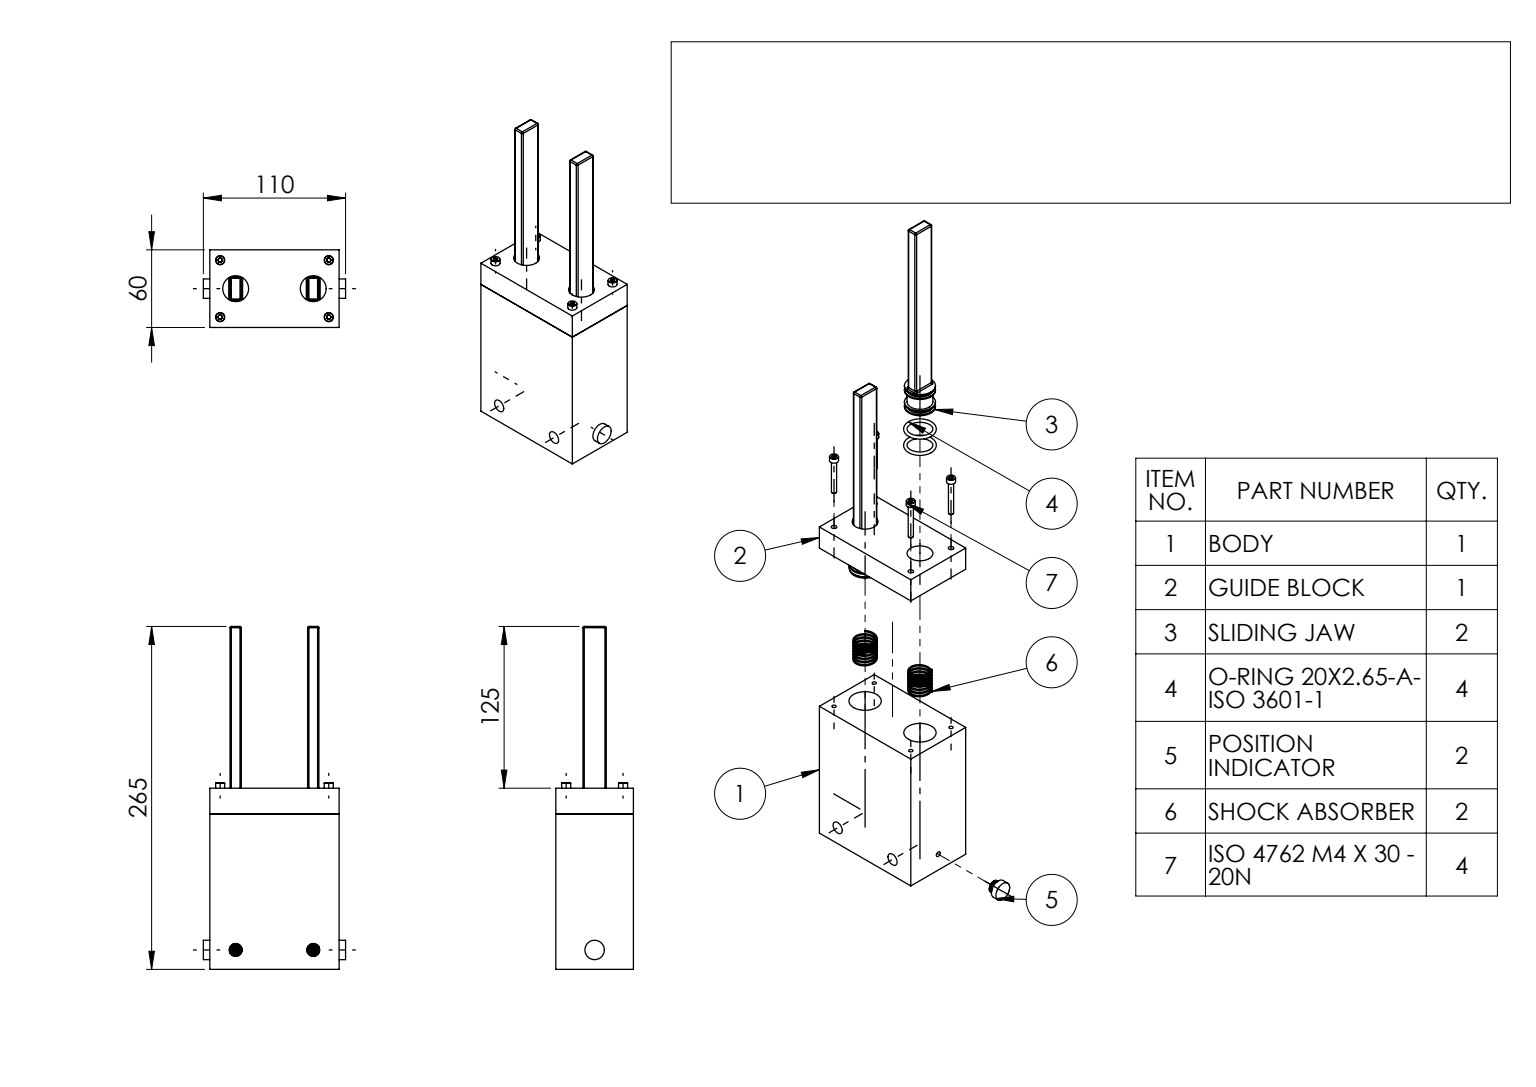
ISO-10303-21;
HEADER;
FILE_DESCRIPTION (('STEP AP214'),
    '1' );
FILE_NAME ('BR-006',
    '2026-09-29T11:11:29',
    ( '' ),
    ( '' ),
    'SwSTEP 2.0',
    'SolidWorks 2026',
    '' );
FILE_SCHEMA (( 'AUTOMOTIVE_DESIGN' ));
ENDSEC;

DATA;
#1 = EDGE_CURVE ( 'NONE', #3439, #1476, #1309, .T. ) ;
#2 = DIRECTION ( 'NONE',  ( 6.123233995736766036E-17, -1.000000000000000000, 0.000000000000000000 ) ) ;
#3 = AXIS2_PLACEMENT_3D ( 'NONE', #1406, #4531, #6990 ) ;
#4 = ORIENTED_EDGE ( 'NONE', *, *, #636, .F. ) ;
#5 = CARTESIAN_POINT ( 'NONE',  ( 42.00000000000000711, 48.00000000000002842, -23.64999999999992042 ) ) ;
#6 = CARTESIAN_POINT ( 'NONE',  ( -39.38303923565386100, -41.70000000000000995, -1.486127417882099788 ) ) ;
#7 = CARTESIAN_POINT ( 'NONE',  ( -22.03669253526174998, -31.34999999999999787, 4.057507815433014642 ) ) ;
#8 = ADVANCED_FACE ( 'NONE', ( #3264 ), #5944, .F. ) ;
#9 = FACE_BOUND ( 'NONE', #6715, .T. ) ;
#10 = FACE_OUTER_BOUND ( 'NONE', #2337, .T. ) ;
#11 = CARTESIAN_POINT ( 'NONE',  ( -21.55948914237271907, -43.89859572486944472, -4.360112732550413206 ) ) ;
#12 = DIRECTION ( 'NONE',  ( 1.000000000000000000, 0.000000000000000000, 0.000000000000000000 ) ) ;
#13 = CARTESIAN_POINT ( 'NONE',  ( 5.000000000000000000, -47.07106781186545419, -99.34999999781506119 ) ) ;
#14 = CARTESIAN_POINT ( 'NONE',  ( -4.566987299999997418, -46.89170807884566727, -96.79999999890753770 ) ) ;
#15 = ORIENTED_EDGE ( 'NONE', *, *, #7694, .T. ) ;
#16 = DIRECTION ( 'NONE',  ( 0.000000000000000000, 0.000000000000000000, 1.000000000000000000 ) ) ;
#17 = CARTESIAN_POINT ( 'NONE',  ( -28.67030704715798350, -46.80000000000001137, 8.395350895058669494 ) ) ;
#18 = CARTESIAN_POINT ( 'NONE',  ( -31.50758917197619979, -41.94859572486944188, 9.874625247442176956 ) ) ;
#19 = CARTESIAN_POINT ( 'NONE',  ( -22.89739904353894318, -38.75140427513058228, -7.023824353025938549 ) ) ;
#20 = PRODUCT_DEFINITION_FORMATION_WITH_SPECIFIED_SOURCE ( 'ANY', '', #288, .NOT_KNOWN. ) ;
#21 = ORIENTED_EDGE ( 'NONE', *, *, #3963, .T. ) ;
#22 = ORIENTED_EDGE ( 'NONE', *, *, #6310, .F. ) ;
#23 = CARTESIAN_POINT ( 'NONE',  ( -21.12512167993187973, -48.35140427513057659, 4.584493831696868860 ) ) ;
#24 = ADVANCED_BREP_SHAPE_REPRESENTATION ( '', ( #85, #2554 ), #7190 ) ;
#25 = DIRECTION ( 'NONE',  ( 1.000000000000000000, 0.000000000000000000, 0.000000000000000000 ) ) ;
#26 = CARTESIAN_POINT ( 'NONE',  ( 5.000000000000000000, -47.07106781186545419, -98.54999999781504982 ) ) ;
#27 = CARTESIAN_POINT ( 'NONE',  ( 3.535533905932737309, -48.53553390593270933, -96.29999999999999716 ) ) ;
#28 = CARTESIAN_POINT ( 'NONE',  ( 9.184850993605145972E-16, -49.99999999999997158, -98.79999999999999716 ) ) ;
#29 = ORIENTED_EDGE ( 'NONE', *, *, #4037, .T. ) ;
#30 = CARTESIAN_POINT ( 'NONE',  ( -22.03669253526174998, -49.35000000000000853, 4.057507815433014642 ) ) ;
#31 = CARTESIAN_POINT ( 'NONE',  ( -23.28248557872775137, -37.50000000000000711, 6.717514421272141156 ) ) ;
#32 = CIRCLE ( 'NONE', #4965, 12.49999999999997335 ) ;
#33 = EDGE_LOOP ( 'NONE', ( #4493, #8102, #3029, #2233, #7688, #6196, #940, #4526, #7806, #8045, #8010, #3978, #7053, #8494, #982 ) ) ;
#34 = CARTESIAN_POINT ( 'NONE',  ( 3.229347689422839895, -41.77065231057713390, -98.94999999890752918 ) ) ;
#35 = CARTESIAN_POINT ( 'NONE',  ( -4.999999999999997335, -47.07106781186546129, -97.24999999781506688 ) ) ;
#36 = CARTESIAN_POINT ( 'NONE',  ( -34.53486167607238144, -42.15000000000001279, -8.900167166472096270 ) ) ;
#37 = CARTESIAN_POINT ( 'NONE',  ( -3.229347689422840784, -41.77065231057713390, -98.54999999890752349 ) ) ;
#38 = CARTESIAN_POINT ( 'NONE',  ( 0.000000000000000000, -44.99999999999997158, -100.0000000000000000 ) ) ;
#39 = STYLED_ITEM ( 'NONE', ( #683 ), #2810 ) ;
#40 = CARTESIAN_POINT ( 'NONE',  ( -28.54686042191934092, -41.45140427513058512, -8.818680382772479120 ) ) ;
#41 = EDGE_CURVE ( 'NONE', #505, #4648, #4851, .T. ) ;
#42 = CARTESIAN_POINT ( 'NONE',  ( -3.535533905932735532, -48.53553390593270933, -98.09300000002185982 ) ) ;
#43 = CARTESIAN_POINT ( 'NONE',  ( -23.68028341417693738, -42.75000000000000711, -6.319716585823200283 ) ) ;
#44 = CARTESIAN_POINT ( 'NONE',  ( 25.66305258423476943, -47.50955795526802206, 11.72510588894413530 ) ) ;
#45 = CARTESIAN_POINT ( 'NONE',  ( -41.99999999999996447, 48.00000000000002842, 22.00000000000000000 ) ) ;
#46 = CONICAL_SURFACE ( 'NONE', #7936, 12.49999999999996980, 1.029744258676651869 ) ;
#47 = CONTEXT_DEPENDENT_SHAPE_REPRESENTATION ( #4249, #7757 ) ;
#48 = EDGE_LOOP ( 'NONE', ( #5523, #4308 ) ) ;
#49 = CARTESIAN_POINT ( 'NONE',  ( -41.99999999999996447, -22.00000000000000000, 80.00000000000002842 ) ) ;
#50 = CARTESIAN_POINT ( 'NONE',  ( -21.09983283352784156, -49.35000000000000853, 4.534861676072186043 ) ) ;
#51 = CARTESIAN_POINT ( 'NONE',  ( -21.17260567462091458, -31.05000000000000782, -1.398121909749242331 ) ) ;
#52 = CIRCLE ( 'NONE', #6511, 10.00000000000000178 ) ;
#53 = CARTESIAN_POINT ( 'NONE',  ( 26.69566991153659785, -41.23356742411069575, 12.05770814628967535 ) ) ;
#54 = DIRECTION ( 'NONE',  ( 1.000000000000000000, 0.000000000000000000, 0.000000000000000000 ) ) ;
#55 = CARTESIAN_POINT ( 'NONE',  ( -23.24502507771338600, -44.49859572486944614, 6.680053920257780220 ) ) ;
#56 = CARTESIAN_POINT ( 'NONE',  ( 4.999999999999998224, -42.92893218813449607, -99.24999999781505267 ) ) ;
#57 = CARTESIAN_POINT ( 'NONE',  ( -21.09983283352783801, -34.35000000000000853, 4.534861676072186043 ) ) ;
#58 = VERTEX_POINT ( 'NONE', #8160 ) ;
#59 = CARTESIAN_POINT ( 'NONE',  ( -33.35889894354067309, -7.999999999999996447, -25.00000000000000000 ) ) ;
#60 = ADVANCED_FACE ( 'NONE', ( #2297 ), #6169, .T. ) ;
#61 = CARTESIAN_POINT ( 'NONE',  ( -34.10713997105786888, -31.14859572486944828, -7.938018618334151455 ) ) ;
#62 = CARTESIAN_POINT ( 'NONE',  ( -25.73429323749904185, -40.59859572486944757, -8.488613101951701267 ) ) ;
#63 = CARTESIAN_POINT ( 'NONE',  ( -31.61762450863942320, -45.95140427513058512, 9.857197362228843573 ) ) ;
#64 = ORIENTED_EDGE ( 'NONE', *, *, #7792, .F. ) ;
#65 = ORIENTED_EDGE ( 'NONE', *, *, #4888, .T. ) ;
#66 = CARTESIAN_POINT ( 'NONE',  ( -22.89739904353894318, -41.75140427513057517, -7.023824353025938549 ) ) ;
#67 = CARTESIAN_POINT ( 'NONE',  ( 42.00000000000000711, -21.99999999999992184, 80.00000000000002842 ) ) ;
#68 = CARTESIAN_POINT ( 'NONE',  ( 4.566987300000000083, -46.89170807884565306, -95.89999999890753202 ) ) ;
#69 = FACE_OUTER_BOUND ( 'NONE', #3093, .T. ) ;
#70 = CARTESIAN_POINT ( 'NONE',  ( -30.00000000000000000, 60.00000000000002842, 0.000000000000000000 ) ) ;
#71 = VERTEX_POINT ( 'NONE', #7660 ) ;
#72 = CARTESIAN_POINT ( 'NONE',  ( -31.38201786482021305, -34.29859572486943620, -8.387063443159975762 ) ) ;
#73 = CARTESIAN_POINT ( 'NONE',  ( -39.86591130483550671, -32.55000000000000426, 1.562606840307984468 ) ) ;
#74 = AXIS2_PLACEMENT_3D ( 'NONE', #4907, #6141, #4116 ) ;
#75 = ORIENTED_EDGE ( 'NONE', *, *, #6394, .T. ) ;
#76 = ADVANCED_FACE ( 'NONE', ( #1450 ), #4832, .F. ) ;
#77 = FACE_OUTER_BOUND ( 'NONE', #632, .T. ) ;
#78 = CARTESIAN_POINT ( 'NONE',  ( -1.891708078845683705, -49.56698729999997255, -97.69999999890751496 ) ) ;
#79 = CARTESIAN_POINT ( 'NONE',  ( -3.535533905932736864, -41.46446609406723383, -95.79999999781504982 ) ) ;
#80 = DIRECTION ( 'NONE',  ( 1.000000000000000000, 0.000000000000000000, 0.000000000000000000 ) ) ;
#81 = CARTESIAN_POINT ( 'NONE',  ( -4.566987299999997418, -46.89170807884566727, -99.99999999890754054 ) ) ;
#82 = CARTESIAN_POINT ( 'NONE',  ( -30.00000000000002842, 0.000000000000000000, -44.00000000000000000 ) ) ;
#83 = AXIS2_PLACEMENT_3D ( 'NONE', #2600, #8057, #1442 ) ;
#84 = CARTESIAN_POINT ( 'NONE',  ( -31.45313957808072303, -39.95140427513058512, 8.818680382772479120 ) ) ;
#85 = MANIFOLD_SOLID_BREP ( '\X2\00d8\X0\20.0 (20) Diameter Hole1', #4490 ) ;
#86 = AXIS2_PLACEMENT_3D ( 'NONE', #4207, #8514, #2479 ) ;
#87 = ADVANCED_FACE ( 'NONE', ( #4979 ), #2915, .F. ) ;
#88 = CARTESIAN_POINT ( 'NONE',  ( -4.999999999999998224, -42.92893218813448897, -96.64300000002185698 ) ) ;
#89 = CIRCLE ( 'NONE', #1214, 3.500000000000000000 ) ;
#90 = UNCERTAINTY_MEASURE_WITH_UNIT (LENGTH_MEASURE( 1.000000000000000082E-05 ), #727, 'distance_accuracy_value', 'NONE');
#91 = CARTESIAN_POINT ( 'NONE',  ( -22.03669253526174998, -43.35000000000000853, 4.057507815433014642 ) ) ;
#92 = DIRECTION ( 'NONE',  ( -0.000000000000000000, 1.000000000000000000, -0.000000000000000000 ) ) ;
#93 = SHAPE_DEFINITION_REPRESENTATION ( #6343, #4062 ) ;
#94 = VERTEX_POINT ( 'NONE', #8292 ) ;
#95 = DIRECTION ( 'NONE',  ( 0.000000000000000000, 0.000000000000000000, -1.000000000000000000 ) ) ;
#96 = CIRCLE ( 'NONE', #1362, 10.00000000000000178 ) ;
#97 = CARTESIAN_POINT ( 'NONE',  ( -25.46513832392765408, -46.65000000000001279, 8.900167166472096270 ) ) ;
#98 = CARTESIAN_POINT ( 'NONE',  ( -34.05750781543318340, -33.15000000000001279, -7.963307464738195840 ) ) ;
#99 = EDGE_CURVE ( 'NONE', #4623, #6070, #4272, .T. ) ;
#100 = CARTESIAN_POINT ( 'NONE',  ( -30.00000000000000000, -40.00000000000002132, 12.49999999999998046 ) ) ;
#101 = CIRCLE ( 'NONE', #1224, 4.999999999999973355 ) ;
#102 = FACE_OUTER_BOUND ( 'NONE', #7927, .T. ) ;
#103 = CARTESIAN_POINT ( 'NONE',  ( -25.73429323749904185, -43.59859572486944046, -8.488613101951701267 ) ) ;
#104 = CARTESIAN_POINT ( 'NONE',  ( -49.99999999999997158, -59.99999999999997158, -30.00000000000000000 ) ) ;
#105 = CARTESIAN_POINT ( 'NONE',  ( -23.28248557872775137, -34.50000000000000000, 6.717514421272141156 ) ) ;
#106 = EDGE_LOOP ( 'NONE', ( #3791, #8082, #1167, #64 ) ) ;
#107 = CARTESIAN_POINT ( 'NONE',  ( 9.184850993605145972E-16, -49.99999999999997158, -98.79999999999999716 ) ) ;
#108 = ORIENTED_EDGE ( 'NONE', *, *, #689, .F. ) ;
#109 = CARTESIAN_POINT ( 'NONE',  ( -25.94249218456686279, -46.65000000000001279, 7.963307464738195840 ) ) ;
#110 = CARTESIAN_POINT ( 'NONE',  ( -31.53845232986046554, -43.29859572486943620, -9.374751783755117529 ) ) ;
#111 = CARTESIAN_POINT ( 'NONE',  ( -36.68005392025794009, -41.00140427513057517, -6.754974922286504757 ) ) ;
#112 = VERTEX_POINT ( 'NONE', #3443 ) ;
#113 = ORIENTED_EDGE ( 'NONE', *, *, #1064, .F. ) ;
#114 = CARTESIAN_POINT ( 'NONE',  ( 4.566987300000000083, -46.89170807884564596, -95.69999999890752918 ) ) ;
#115 = CARTESIAN_POINT ( 'NONE',  ( -23.28248557872775137, -31.50000000000000711, 6.717514421272141156 ) ) ;
#116 = CARTESIAN_POINT ( 'NONE',  ( 0.000000000000000000, -44.99999999999997158, -95.00000000000000000 ) ) ;
#117 = CARTESIAN_POINT ( 'NONE',  ( 3.229347689422841228, -48.22934768942280925, -96.74999999890751212 ) ) ;
#118 = CARTESIAN_POINT ( 'NONE',  ( -26.64110105645932336, -7.999999999999996447, -23.99999999999999289 ) ) ;
#119 = FACE_OUTER_BOUND ( 'NONE', #8547, .T. ) ;
#120 = VERTEX_POINT ( 'NONE', #6909 ) ;
#121 = CARTESIAN_POINT ( 'NONE',  ( -33.85891924778610473, -50.10000000000000853, 7.573555455601171715 ) ) ;
#122 = CARTESIAN_POINT ( 'NONE',  ( -25.46513832392765408, -31.65000000000000568, 8.900167166472096270 ) ) ;
#123 = ORIENTED_EDGE ( 'NONE', *, *, #7045, .T. ) ;
#124 = CARTESIAN_POINT ( 'NONE',  ( -20.13408869516453947, -46.05000000000001137, -1.562606840307983136 ) ) ;
#125 = DIRECTION ( 'NONE',  ( -0.000000000000000000, 1.000000000000000000, -0.000000000000000000 ) ) ;
#126 = CARTESIAN_POINT ( 'NONE',  ( 1.891708078845685481, -49.56698729999997255, -96.79999999890752349 ) ) ;
#127 = CARTESIAN_POINT ( 'NONE',  ( -3.061616997868382155E-16, -39.99999999999997158, -100.6999999978150555 ) ) ;
#128 = CARTESIAN_POINT ( 'NONE',  ( -30.00000000000002842, 0.000000000000000000, -45.00000000000000000 ) ) ;
#129 = CARTESIAN_POINT ( 'NONE',  ( 4.566987299999998307, -44.99999999999997158, -98.04999999890752349 ) ) ;
#130 = EDGE_CURVE ( 'NONE', #858, #6099, #1687, .T. ) ;
#131 = CARTESIAN_POINT ( 'NONE',  ( -38.83610826798580717, -46.55140427513058654, 1.343104241417631073 ) ) ;
#132 = CARTESIAN_POINT ( 'NONE',  ( -3.061616997868382155E-16, -39.99999999999997158, -98.39300000002185698 ) ) ;
#133 = CARTESIAN_POINT ( 'NONE',  ( 4.566987300000000083, -46.89170807884565306, -95.69999999890755760 ) ) ;
#134 = CARTESIAN_POINT ( 'NONE',  ( -31.32969295284206979, -48.30000000000001137, -8.395350895058669494 ) ) ;
#135 = CIRCLE ( 'NONE', #6335, 3.299999999999999822 ) ;
#136 = CARTESIAN_POINT ( 'NONE',  ( 0.000000000000000000, 0.8865213383406683745, -1.535500000000000753 ) ) ;
#137 = EDGE_CURVE ( 'NONE', #5904, #1249, #6293, .T. ) ;
#138 = APPLICATION_PROTOCOL_DEFINITION ( 'draft international standard', 'automotive_design', 1998, #7229 ) ;
#139 = EDGE_LOOP ( 'NONE', ( #1708, #6887, #7126, #967 ) ) ;
#140 = CARTESIAN_POINT ( 'NONE',  ( 0.000000000000000000, 0.000000000000000000, -30.00000000000000000 ) ) ;
#141 = DIRECTION ( 'NONE',  ( 0.000000000000000000, 0.000000000000000000, 1.000000000000000000 ) ) ;
#142 = CARTESIAN_POINT ( 'NONE',  ( -25.94249218456686279, -34.64999999999998437, 7.963307464738195840 ) ) ;
#143 = CIRCLE ( 'NONE', #4647, 9.999999999999998224 ) ;
#144 = CARTESIAN_POINT ( 'NONE',  ( -25.51828610110682405, -42.77717578641267693, 11.66923617342549413 ) ) ;
#145 = CARTESIAN_POINT ( 'NONE',  ( 45.00000000000003553, -44.99999999999997158, 0.000000000000000000 ) ) ;
#146 = CARTESIAN_POINT ( 'NONE',  ( -34.58449383169706692, -46.14859572486944472, -8.874878320068054549 ) ) ;
#147 = CARTESIAN_POINT ( 'NONE',  ( 1.308739421796400793, -40.13013661665839038, -99.99999999999998579 ) ) ;
#148 = CARTESIAN_POINT ( 'NONE',  ( -20.61696076434619584, -34.20000000000000995, 1.486127417882100676 ) ) ;
#149 =( NAMED_UNIT ( * ) PLANE_ANGLE_UNIT ( ) SI_UNIT ( $, .RADIAN. ) );
#150 = EDGE_LOOP ( 'NONE', ( #1097, #2734, #1435, #2240, #218 ) ) ;
#151 = LINE ( 'NONE', #8229, #3888 ) ;
#152 = ORIENTED_EDGE ( 'NONE', *, *, #4060, .F. ) ;
#153 = CARTESIAN_POINT ( 'NONE',  ( -21.59636165304264921, -38.19859572486942767, 1.277368040863740228 ) ) ;
#154 = ADVANCED_FACE ( 'NONE', ( #77 ), #1363, .T. ) ;
#155 = CARTESIAN_POINT ( 'NONE',  ( -21.07454398712378918, -44.34859572486944046, 4.485229520447505003 ) ) ;
#156 = CARTESIAN_POINT ( 'NONE',  ( -39.37475178375516549, -43.70140427513058512, -1.538452329860249712 ) ) ;
#157 = CIRCLE ( 'NONE', #7186, 11.99999999999979217 ) ;
#158 = EDGE_CURVE ( 'NONE', #8668, #1053, #2208, .T. ) ;
#159 = EDGE_LOOP ( 'NONE', ( #5400, #1966 ) ) ;
#160 = CARTESIAN_POINT ( 'NONE',  ( 3.229347689422841228, -48.22934768942280925, -97.34999999890753486 ) ) ;
#161 = DIRECTION ( 'NONE',  ( 0.000000000000000000, 0.000000000000000000, 1.000000000000000000 ) ) ;
#162 = CARTESIAN_POINT ( 'NONE',  ( -30.00000000000002842, 0.000000000000000000, -28.65000000000000213 ) ) ;
#163 = CARTESIAN_POINT ( 'NONE',  ( -4.566987299999997418, -46.89170807884566727, -98.59999999890753486 ) ) ;
#164 = CARTESIAN_POINT ( 'NONE',  ( -30.00000000000002487, 0.000000000000000000, -25.00000000000000000 ) ) ;
#165 = DIRECTION ( 'NONE',  ( -0.000000000000000000, -0.000000000000000000, -1.000000000000000000 ) ) ;
#166 = EDGE_LOOP ( 'NONE', ( #6634, #5758, #5300, #3325 ) ) ;
#167 = CARTESIAN_POINT ( 'NONE',  ( -38.81868038277247734, -36.54859572486943620, 1.453139578080855365 ) ) ;
#168 = CARTESIAN_POINT ( 'NONE',  ( -36.71751442127229836, -30.00000000000000711, -6.717514421272142044 ) ) ;
#169 = EDGE_LOOP ( 'NONE', ( #3481, #7886, #4, #4040 ) ) ;
#170 = CARTESIAN_POINT ( 'NONE',  ( -25.68709025247441602, -48.60000000000000142, -8.464561979789547053 ) ) ;
#171 =( GEOMETRIC_REPRESENTATION_CONTEXT ( 3 ) GLOBAL_UNCERTAINTY_ASSIGNED_CONTEXT ( ( #1678 ) ) GLOBAL_UNIT_ASSIGNED_CONTEXT ( ( #6656, #613, #5915 ) ) REPRESENTATION_CONTEXT ( 'NONE', 'WORKASPACE' ) );
#172 = CARTESIAN_POINT ( 'NONE',  ( -2.071067811865475505, -49.99999999999997158, -98.74999999781503845 ) ) ;
#173 = CARTESIAN_POINT ( 'NONE',  ( -3.229347689422839451, -48.22934768942280925, -100.1499999989075178 ) ) ;
#174 = CARTESIAN_POINT ( 'NONE',  ( 5.000000000000000000, -47.07106781186545419, -98.54999999781504982 ) ) ;
#175 = CARTESIAN_POINT ( 'NONE',  ( 0.000000000000000000, -44.99999999999997158, -100.0000000000000000 ) ) ;
#176 = CARTESIAN_POINT ( 'NONE',  ( 4.566987300000000083, -46.89170807884565306, -97.29999999890750928 ) ) ;
#177 = ADVANCED_FACE ( 'NONE', ( #4445 ), #1804, .F. ) ;
#178 = CARTESIAN_POINT ( 'NONE',  ( -23.64089511245930098, -44.75140427513058228, -6.280328284105564762 ) ) ;
#179 = CARTESIAN_POINT ( 'NONE',  ( 4.999999999999998224, -42.92893218813448897, -99.34300000002184561 ) ) ;
#180 = CARTESIAN_POINT ( 'NONE',  ( -1.891708078845683039, -40.43301269999998482, -96.19999999890752918 ) ) ;
#181 = PRESENTATION_LAYER_ASSIGNMENT (  '', '', ( #3433 ) ) ;
#182 = CARTESIAN_POINT ( 'NONE',  ( -23.68028341417693738, -48.75000000000000711, -6.319716585823200283 ) ) ;
#183 = CARTESIAN_POINT ( 'NONE',  ( -30.00000000000002842, 10.00000000000000178, -24.00000000000000000 ) ) ;
#184 = LINE ( 'NONE', #7585, #2081 ) ;
#185 = CARTESIAN_POINT ( 'NONE',  ( -21.60464910494133406, -37.20000000000000284, 1.329692952841886155 ) ) ;
#186 = STYLED_ITEM ( 'NONE', ( #5619 ), #2959 ) ;
#187 = CARTESIAN_POINT ( 'NONE',  ( 29.34107419296792685, -40.03249052150653142, 12.48689449661282858 ) ) ;
#188 = EDGE_CURVE ( 'NONE', #5393, #2290, #961, .T. ) ;
#189 = CYLINDRICAL_SURFACE ( 'NONE', #1544, 4.999999999999998224 ) ;
#190 = CARTESIAN_POINT ( 'NONE',  ( -38.44051085762733777, -45.39859572486944472, 4.360112732550414982 ) ) ;
#191 = DIRECTION ( 'NONE',  ( -0.000000000000000000, 0.000000000000000000, 1.000000000000000000 ) ) ;
#192 = CARTESIAN_POINT ( 'NONE',  ( -34.31290974752564438, -32.10000000000000142, 8.464561979789547053 ) ) ;
#193 =( REPRESENTATION_RELATIONSHIP ('NONE','NONE', #2265, #6471 ) REPRESENTATION_RELATIONSHIP_WITH_TRANSFORMATION ( #6877 )SHAPE_REPRESENTATION_RELATIONSHIP( ) );
#194 = ORIENTED_EDGE ( 'NONE', *, *, #7448, .F. ) ;
#195 = CARTESIAN_POINT ( 'NONE',  ( -33.35889894354067309, -9.999999999999998224, -25.00000000000000000 ) ) ;
#196 = VERTEX_POINT ( 'NONE', #4485 ) ;
#197 = CARTESIAN_POINT ( 'NONE',  ( -26.18828373723858149, -43.59859572486944046, -7.597606577763319713 ) ) ;
#198 = CARTESIAN_POINT ( 'NONE',  ( -25.68709025247441602, -30.60000000000000142, -8.464561979789547053 ) ) ;
#199 = CARTESIAN_POINT ( 'NONE',  ( -38.83610826798580717, -31.55140427513057588, 1.343104241417631073 ) ) ;
#200 = EDGE_LOOP ( 'NONE', ( #2778, #541, #7748, #7443, #585 ) ) ;
#201 = CARTESIAN_POINT ( 'NONE',  ( -4.566987299999998307, -43.10829192115428299, -96.09999999890753486 ) ) ;
#202 = SURFACE_STYLE_FILL_AREA ( #243 ) ;
#203 = FACE_BOUND ( 'NONE', #7034, .T. ) ;
#204 = CARTESIAN_POINT ( 'NONE',  ( 4.566987299999998307, -44.99999999999997158, -99.04999999890752349 ) ) ;
#205 = CARTESIAN_POINT ( 'NONE',  ( -25.16271839757670747, -46.30802241892378390, 11.52630626327735364 ) ) ;
#206 = DIRECTION ( 'NONE',  ( -1.000000000000000000, 0.000000000000000000, 0.000000000000000000 ) ) ;
#207 = VERTEX_POINT ( 'NONE', #7881 ) ;
#208 = CARTESIAN_POINT ( 'NONE',  ( -31.38201786482021305, -46.29859572486944330, -8.387063443159975762 ) ) ;
#209 = CARTESIAN_POINT ( 'NONE',  ( -34.31290974752564438, -41.10000000000000142, 8.464561979789547053 ) ) ;
#210 = ORIENTED_EDGE ( 'NONE', *, *, #267, .T. ) ;
#211 = CARTESIAN_POINT ( 'NONE',  ( -36.71751442127229836, -45.00000000000000711, -6.717514421272142044 ) ) ;
#212 = SURFACE_SIDE_STYLE ('',( #6821 ) ) ;
#213 = CARTESIAN_POINT ( 'NONE',  ( 4.999999999999998224, -44.99999999999997158, -98.60000000000000853 ) ) ;
#214 = ADVANCED_FACE ( 'NONE', ( #3002 ), #7128, .T. ) ;
#215 = CARTESIAN_POINT ( 'NONE',  ( -3.535533905932735532, -48.53553390593270933, -100.3999999978150441 ) ) ;
#216 = LINE ( 'NONE', #4229, #1862 ) ;
#217 = CARTESIAN_POINT ( 'NONE',  ( -3.229347689422840784, -41.77065231057713390, -99.34999999890753486 ) ) ;
#218 = ORIENTED_EDGE ( 'NONE', *, *, #2863, .T. ) ;
#219 = CARTESIAN_POINT ( 'NONE',  ( -37.93801861833426159, -40.85140427513057659, -4.107139971057695682 ) ) ;
#220 = AXIS2_PLACEMENT_3D ( 'NONE', #5235, #7767, #7308 ) ;
#221 = CARTESIAN_POINT ( 'NONE',  ( 9.184850993605145972E-16, -49.99999999999997158, -99.59300000002184561 ) ) ;
#222 = CYLINDRICAL_SURFACE ( 'NONE', #8532, 1.000000000000000888 ) ;
#223 = CARTESIAN_POINT ( 'NONE',  ( -28.67030704715798350, -46.80000000000001137, 8.395350895058669494 ) ) ;
#224 = LINE ( 'NONE', #3711, #2134 ) ;
#225 = ITEM_DEFINED_TRANSFORMATION ( 'NONE', 'NONE', #3556,  #2554 ) ;
#226 = DIRECTION ( 'NONE',  ( -0.000000000000000000, -0.000000000000000000, -1.000000000000000000 ) ) ;
#227 = CARTESIAN_POINT ( 'NONE',  ( -23.68028341417693738, -42.75000000000001421, -6.319716585823198507 ) ) ;
#228 = CARTESIAN_POINT ( 'NONE',  ( 25.51351754887333101, -42.76835092305877595, 11.66791272636411847 ) ) ;
#229 = CYLINDRICAL_SURFACE ( 'NONE', #3390, 10.00000000000000178 ) ;
#230 = CARTESIAN_POINT ( 'NONE',  ( -34.53486167607238144, -33.15000000000001279, -8.900167166472096270 ) ) ;
#231 = CARTESIAN_POINT ( 'NONE',  ( -30.00000000000000000, 0.000000000000000000, 80.00000000000002842 ) ) ;
#232 = CARTESIAN_POINT ( 'NONE',  ( -21.53543802021056663, -36.90000000000000568, -4.312909747525783821 ) ) ;
#233 = SURFACE_SIDE_STYLE ('',( #7637 ) ) ;
#234 = EDGE_LOOP ( 'NONE', ( #2783, #7992, #7432, #4971 ) ) ;
#235 = CARTESIAN_POINT ( 'NONE',  ( 50.00000000000002842, -44.99999999999997158, 0.000000000000000000 ) ) ;
#236 = ORIENTED_EDGE ( 'NONE', *, *, #746, .T. ) ;
#237 = CARTESIAN_POINT ( 'NONE',  ( -22.45049566656107842, -40.89859572486943762, -3.906122232810846917 ) ) ;
#238 = CARTESIAN_POINT ( 'NONE',  ( -21.53543802021056663, -30.90000000000000924, -4.312909747525783821 ) ) ;
#239 = CARTESIAN_POINT ( 'NONE',  ( -36.68005392025794009, -47.00140427513058938, -6.754974922286504757 ) ) ;
#240 = AXIS2_PLACEMENT_3D ( 'NONE', #1947, #6742, #7321 ) ;
#241 = CARTESIAN_POINT ( 'NONE',  ( 4.566987299999998307, -44.99999999999997158, -95.64999999890753202 ) ) ;
#242 =( GEOMETRIC_REPRESENTATION_CONTEXT ( 3 ) GLOBAL_UNCERTAINTY_ASSIGNED_CONTEXT ( ( #3453 ) ) GLOBAL_UNIT_ASSIGNED_CONTEXT ( ( #4314, #5632, #8331 ) ) REPRESENTATION_CONTEXT ( 'NONE', 'WORKASPACE' ) );
#243 = FILL_AREA_STYLE ('',( #6897 ) ) ;
#244 = PLANE ( 'NONE',  #7417 ) ;
#245 = CARTESIAN_POINT ( 'NONE',  ( -3.229347689422840784, -41.77065231057713390, -96.34999999890752065 ) ) ;
#246 = CARTESIAN_POINT ( 'NONE',  ( 4.999999999999998224, -44.99999999999997158, -95.40000000000000568 ) ) ;
#247 = CARTESIAN_POINT ( 'NONE',  ( -49.99999999999997158, 60.00000000000002842, 30.00000000000000000 ) ) ;
#248 = FACE_OUTER_BOUND ( 'NONE', #8420, .T. ) ;
#249 = ORIENTED_EDGE ( 'NONE', *, *, #158, .T. ) ;
#250 = EDGE_CURVE ( 'NONE', #6544, #5958, #4898, .T. ) ;
#251 = CARTESIAN_POINT ( 'NONE',  ( -37.98859631114233792, -39.84859572486944046, -4.007875659808334490 ) ) ;
#252 = CARTESIAN_POINT ( 'NONE',  ( -25.46513832392765408, -43.64999999999999147, 8.900167166472096270 ) ) ;
#253 = ORIENTED_EDGE ( 'NONE', *, *, #4306, .F. ) ;
#254 = CARTESIAN_POINT ( 'NONE',  ( -34.48522952044771017, -29.15140427513058441, -8.925456012876139766 ) ) ;
#255 = DIRECTION ( 'NONE',  ( -1.000000000000000000, -0.000000000000000000, -0.000000000000000000 ) ) ;
#256 = CARTESIAN_POINT ( 'NONE',  ( -3.535533905932736864, -41.46446609406723383, -100.5999999978150470 ) ) ;
#257 = EDGE_CURVE ( 'NONE', #6677, #2955, #1349, .T. ) ;
#258 = CARTESIAN_POINT ( 'NONE',  ( -4.999999999999998224, -44.99999999999997158, -98.09999999781504698 ) ) ;
#259 = CARTESIAN_POINT ( 'NONE',  ( -3.229347689422839451, -48.22934768942280925, -98.34999999890753486 ) ) ;
#260 = ORIENTED_EDGE ( 'NONE', *, *, #8374, .T. ) ;
#261 = CARTESIAN_POINT ( 'NONE',  ( -25.94249218456686279, -34.64999999999998437, 7.963307464738195840 ) ) ;
#262 = PRODUCT_DEFINITION_SHAPE ( 'NONE', 'NONE',  #8722 ) ;
#263 = VECTOR ( 'NONE', #3964, 1000.000000000000227 ) ;
#264 = CARTESIAN_POINT ( 'NONE',  ( 3.535533905932736420, -41.46446609406723383, -95.29999999999999716 ) ) ;
#265 = FACE_OUTER_BOUND ( 'NONE', #169, .T. ) ;
#266 = CARTESIAN_POINT ( 'NONE',  ( -36.01040764008574513, -51.00000000000000711, -6.010407640085605685 ) ) ;
#267 = EDGE_CURVE ( 'NONE', #4999, #1695, #7837, .T. ) ;
#268 = DIRECTION ( 'NONE',  ( -0.000000000000000000, 1.000000000000000000, -0.000000000000000000 ) ) ;
#269 = CARTESIAN_POINT ( 'NONE',  ( 4.999999999999998224, -42.92893218813449607, -100.0499999978150640 ) ) ;
#270 = CARTESIAN_POINT ( 'NONE',  ( -22.42644454439892598, -36.90000000000000568, -3.858919247786222861 ) ) ;
#271 = PRODUCT_RELATED_PRODUCT_CATEGORY ( 'part', '', ( #3671 ) ) ;
#272 = CARTESIAN_POINT ( 'NONE',  ( -1.891708078845683039, -40.43301269999998482, -95.59999999890753486 ) ) ;
#273 = DIRECTION ( 'NONE',  ( -0.000000000000000000, -0.000000000000000000, 1.000000000000000000 ) ) ;
#274 = CARTESIAN_POINT ( 'NONE',  ( -37.06321265474346660, -32.25000000000000711, 7.063212654743582952 ) ) ;
#275 = EDGE_CURVE ( 'NONE', #5958, #6544, #655, .T. ) ;
#276 = CARTESIAN_POINT ( 'NONE',  ( -30.00000000000002487, 0.000000000000000000, -40.35000000000000142 ) ) ;
#277 = CARTESIAN_POINT ( 'NONE',  ( -23.28248557872775137, -43.50000000000001421, 6.717514421272141156 ) ) ;
#278 = SURFACE_STYLE_FILL_AREA ( #8401 ) ;
#279 = ORIENTED_EDGE ( 'NONE', *, *, #4946, .T. ) ;
#280 = DIRECTION ( 'NONE',  ( 1.000000000000000000, 0.000000000000000000, 0.000000000000000000 ) ) ;
#281 = ADVANCED_FACE ( 'NONE', ( #6423 ), #7751, .T. ) ;
#282 = VERTEX_POINT ( 'NONE', #3656 ) ;
#283 = CARTESIAN_POINT ( 'NONE',  ( -33.81171626276147890, -39.09859572486944046, 7.597606577763319713 ) ) ;
#284 = CARTESIAN_POINT ( 'NONE',  ( -31.50758917197619979, -50.94859572486944899, 9.874625247442176956 ) ) ;
#285 = CARTESIAN_POINT ( 'NONE',  ( -26.09387776718931917, -29.60140427513057659, -7.549504333439021941 ) ) ;
#286 = CARTESIAN_POINT ( 'NONE',  ( 1.891708078845682595, -40.43301269999998482, -97.89999999890753202 ) ) ;
#287 =( NAMED_UNIT ( * ) SI_UNIT ( $, .STERADIAN. ) SOLID_ANGLE_UNIT ( ) );
#288 = PRODUCT ( 'o-rings series a_iso_O-ring 20x2.65-A-ISO 3601-1', 'o-rings series a_iso_O-ring 20x2.65-A-ISO 3601-1', '', ( #6267 ) ) ;
#289 = CARTESIAN_POINT ( 'NONE',  ( 3.229347689422839895, -41.77065231057713390, -96.54999999890752349 ) ) ;
#290 = FACE_OUTER_BOUND ( 'NONE', #2679, .T. ) ;
#291 = CARTESIAN_POINT ( 'NONE',  ( -3.229347689422839451, -48.22934768942280925, -98.54999999890752349 ) ) ;
#292 = FACE_OUTER_BOUND ( 'NONE', #3738, .T. ) ;
#293 = EDGE_LOOP ( 'NONE', ( #5848, #7323 ) ) ;
#294 = CARTESIAN_POINT ( 'NONE',  ( -23.71967171589458445, -40.74859572486943904, -6.359104887540838469 ) ) ;
#295 = CARTESIAN_POINT ( 'NONE',  ( -38.46456197978948666, -41.40000000000000568, 4.312909747525784709 ) ) ;
#296 =( GEOMETRIC_REPRESENTATION_CONTEXT ( 3 ) GLOBAL_UNCERTAINTY_ASSIGNED_CONTEXT ( ( #1750 ) ) GLOBAL_UNIT_ASSIGNED_CONTEXT ( ( #6287, #2077, #6826 ) ) REPRESENTATION_CONTEXT ( 'NONE', 'WORKASPACE' ) );
#297 = EDGE_LOOP ( 'NONE', ( #7716, #333, #3919, #4177, #5787 ) ) ;
#298 = CARTESIAN_POINT ( 'NONE',  ( -21.12512167993187973, -30.35140427513058015, 4.584493831696868860 ) ) ;
#299 = DIRECTION ( 'NONE',  ( -1.000000000000000000, 0.000000000000000000, 0.000000000000000000 ) ) ;
#300 = DIRECTION ( 'NONE',  ( 0.000000000000000000, 0.000000000000000000, 1.000000000000000000 ) ) ;
#301 = CARTESIAN_POINT ( 'NONE',  ( 9.184850993605145972E-16, -49.99999999999997158, -100.2999999978150498 ) ) ;
#302 = STYLED_ITEM ( 'NONE', ( #2499 ), #2657 ) ;
#303 = DIRECTION ( 'NONE',  ( -0.000000000000000000, -0.000000000000000000, -1.000000000000000000 ) ) ;
#304 = CARTESIAN_POINT ( 'NONE',  ( -3.229347689422840784, -41.77065231057713390, -100.1499999989075320 ) ) ;
#305 = ORIENTED_EDGE ( 'NONE', *, *, #5462, .T. ) ;
#306 = CARTESIAN_POINT ( 'NONE',  ( -33.85891924778610473, -35.10000000000000853, 7.573555455601171715 ) ) ;
#307 = AXIS2_PLACEMENT_3D ( 'NONE', #1866, #1194, #4023 ) ;
#308 = CARTESIAN_POINT ( 'NONE',  ( -4.999999999999998224, -45.95670858091268940, -94.97690301168722726 ) ) ;
#310 = CIRCLE ( 'NONE', #7910, 0.5000000000000001110 ) ;
#309 = CARTESIAN_POINT ( 'NONE',  ( -1.891708078845683483, -49.56698729999997255, -95.89999999890753202 ) ) ;
#311 = CARTESIAN_POINT ( 'NONE',  ( -2.071067811865475061, -39.99999999999997158, -96.64999999781504414 ) ) ;
#312 = AXIS2_PLACEMENT_3D ( 'NONE', #7185, #3059, #1145 ) ;
#313 = CARTESIAN_POINT ( 'NONE',  ( 50.00000000000002842, -44.99999999999997158, 0.000000000000000000 ) ) ;
#314 = CARTESIAN_POINT ( 'NONE',  ( -38.39535089505872634, -35.70000000000000995, -1.329692952841885267 ) ) ;
#315 = AXIS2_PLACEMENT_3D ( 'NONE', #2642, #5313, #2599 ) ;
#316 = CARTESIAN_POINT ( 'NONE',  ( -39.84999999999998010, -22.00000000000000000, 80.00000000000002842 ) ) ;
#317 = CARTESIAN_POINT ( 'NONE',  ( 39.85000000000002274, 21.99999999999992184, 60.00000000000002842 ) ) ;
#318 = CARTESIAN_POINT ( 'NONE',  ( -25.46513832392765408, -37.65000000000000568, 8.900167166472096270 ) ) ;
#319 = CARTESIAN_POINT ( 'NONE',  ( -26.64110105645932336, -7.999999999999996447, 125.0000000000000000 ) ) ;
#320 = CARTESIAN_POINT ( 'NONE',  ( -37.06321265474346660, -44.25000000000000000, 7.063212654743582952 ) ) ;
#321 =( NAMED_UNIT ( * ) PLANE_ANGLE_UNIT ( ) SI_UNIT ( $, .RADIAN. ) );
#322 = EDGE_LOOP ( 'NONE', ( #8677, #7395, #7387, #6062 ) ) ;
#323 = ORIENTED_EDGE ( 'NONE', *, *, #6329, .F. ) ;
#324 = CARTESIAN_POINT ( 'NONE',  ( -34.10713997105786888, -43.14859572486943762, -7.938018618334151455 ) ) ;
#325 = CARTESIAN_POINT ( 'NONE',  ( -28.49241082802385350, -49.44859572486943478, -9.874625247442173404 ) ) ;
#326 = CARTESIAN_POINT ( 'NONE',  ( -37.59760657776328685, -31.40140427513058086, 3.811716262761598362 ) ) ;
#327 = CARTESIAN_POINT ( 'NONE',  ( 42.00000000000000711, 60.00000000000002842, -20.34999999999992326 ) ) ;
#328 = CARTESIAN_POINT ( 'NONE',  ( 25.00000000000004263, -44.99999999999995737, 11.45643923738958314 ) ) ;
#329 = CARTESIAN_POINT ( 'NONE',  ( -21.09983283352784156, -40.35000000000000142, 4.534861676072186043 ) ) ;
#330 = CARTESIAN_POINT ( 'NONE',  ( 3.229347689422841228, -48.22934768942280925, -99.94999999890752918 ) ) ;
#331 = SPHERICAL_SURFACE ( 'NONE', #3585, 1.000000000000000000 ) ;
#332 = CARTESIAN_POINT ( 'NONE',  ( 1.891708078845682595, -40.43301269999998482, -95.69999999890751496 ) ) ;
#333 = ORIENTED_EDGE ( 'NONE', *, *, #6376, .F. ) ;
#334 = CARTESIAN_POINT ( 'NONE',  ( -22.01140368885771892, -38.34859572486944046, 4.007875659808335378 ) ) ;
#335 = AXIS2_PLACEMENT_3D ( 'NONE', #4090, #3522, #8324 ) ;
#336 = CARTESIAN_POINT ( 'NONE',  ( -22.93678734525658314, -42.75000000000001421, -7.063212654743582952 ) ) ;
#337 = ORIENTED_EDGE ( 'NONE', *, *, #267, .F. ) ;
#338 = CARTESIAN_POINT ( 'NONE',  ( -25.51477047955235378, -39.65140427513058086, 8.925456012876139766 ) ) ;
#339 = DIRECTION ( 'NONE',  ( -1.000000000000000000, 0.000000000000000000, 0.000000000000000000 ) ) ;
#340 = CARTESIAN_POINT ( 'NONE',  ( -26.64110105645932336, 8.000000000000000000, 124.0000000000000000 ) ) ;
#341 = CARTESIAN_POINT ( 'NONE',  ( -2.995331045737738095E-16, -40.10825317499996601, -100.0624999997268958 ) ) ;
#342 = DIRECTION ( 'NONE',  ( -1.000000000000000000, 0.000000000000000000, 0.000000000000000000 ) ) ;
#343 = CARTESIAN_POINT ( 'NONE',  ( 2.071067811865474173, -39.99999999999997158, -96.85000000000002274 ) ) ;
#344 = VERTEX_POINT ( 'NONE', #379 ) ;
#345 = CARTESIAN_POINT ( 'NONE',  ( -26.14108075221394856, -30.60000000000000142, -7.573555455601170827 ) ) ;
#346 = ORIENTED_EDGE ( 'NONE', *, *, #5233, .F. ) ;
#347 = CARTESIAN_POINT ( 'NONE',  ( 3.535533905932736420, -41.46446609406723383, -97.69999999999998863 ) ) ;
#348 = CARTESIAN_POINT ( 'NONE',  ( 4.999999999999998224, -42.92893218813448897, -96.84999999781504698 ) ) ;
#349 = CARTESIAN_POINT ( 'NONE',  ( 42.00000000000000711, 60.00000000000002842, -21.99999999999992184 ) ) ;
#350 = LINE ( 'NONE', #3185, #3142 ) ;
#351 = ADVANCED_FACE ( 'NONE', ( #3786 ), #5764, .T. ) ;
#352 = CARTESIAN_POINT ( 'NONE',  ( -36.31971658582311591, -44.25000000000000000, 6.319716585823199395 ) ) ;
#353 = PRODUCT_DEFINITION_SHAPE ( 'NONE', 'NONE',  #8719 ) ;
#354 = CARTESIAN_POINT ( 'NONE',  ( -4.999999999999997335, -47.07106781186546129, -97.24999999781505267 ) ) ;
#355 = CARTESIAN_POINT ( 'NONE',  ( -4.566987299999998307, -44.99999999999997158, -95.24999999890752633 ) ) ;
#356 = DIRECTION ( 'NONE',  ( 0.000000000000000000, 0.000000000000000000, 1.000000000000000000 ) ) ;
#357 = CARTESIAN_POINT ( 'NONE',  ( -21.53543802021056663, -36.90000000000000568, -4.312909747525783821 ) ) ;
#358 = DIRECTION ( 'NONE',  ( -0.000000000000000000, 1.000000000000000000, -0.000000000000000000 ) ) ;
#359 = CARTESIAN_POINT ( 'NONE',  ( -25.68709025247441602, -36.60000000000000853, -8.464561979789547053 ) ) ;
#360 = EDGE_LOOP ( 'NONE', ( #4155, #3028, #6612 ) ) ;
#361 = CARTESIAN_POINT ( 'NONE',  ( -36.04786814110010340, -51.99859572486943193, -5.972947139071243861 ) ) ;
#362 = CARTESIAN_POINT ( 'NONE',  ( -20.61696076434619584, -31.20000000000000639, 1.486127417882100676 ) ) ;
#363 = CARTESIAN_POINT ( 'NONE',  ( -23.64089511245930098, -32.75140427513057517, -6.280328284105564762 ) ) ;
#364 = ADVANCED_FACE ( 'NONE', ( #6505 ), #5809, .T. ) ;
#365 = CARTESIAN_POINT ( 'NONE',  ( -4.566987299999998307, -43.10829192115428299, -99.29999999890752349 ) ) ;
#366 = DIRECTION ( 'NONE',  ( 0.000000000000000000, 0.000000000000000000, 1.000000000000000000 ) ) ;
#367 = CARTESIAN_POINT ( 'NONE',  ( -21.53543802021056663, -33.90000000000000568, -4.312909747525783821 ) ) ;
#368 = AXIS2_PLACEMENT_3D ( 'NONE', #2667, #5963, #5335 ) ;
#369 = CARTESIAN_POINT ( 'NONE',  ( -36.01040764008574513, -30.00000000000000711, -6.010407640085605685 ) ) ;
#370 = CARTESIAN_POINT ( 'NONE',  ( -31.74999999999995737, 0.000000000000000000, 2.000000000000000888 ) ) ;
#371 = CARTESIAN_POINT ( 'NONE',  ( 4.566987299999998307, -44.99999999999997158, -98.24999999890751212 ) ) ;
#372 =( LENGTH_UNIT ( ) NAMED_UNIT ( * ) SI_UNIT ( .MILLI., .METRE. ) );
#373 = ORIENTED_EDGE ( 'NONE', *, *, #4139, .T. ) ;
#374 = CARTESIAN_POINT ( 'NONE',  ( -37.54950433343896776, -45.39859572486944472, 3.906122232810848249 ) ) ;
#375 = CARTESIAN_POINT ( 'NONE',  ( -31.48612741788231517, -45.30000000000000426, -9.383039235653804155 ) ) ;
#376 = TOROIDAL_SURFACE ( 'NONE', #3209, 2.200000000000001066, 0.2000000000000000111 ) ;
#377 = ORIENTED_EDGE ( 'NONE', *, *, #4137, .F. ) ;
#378 = CARTESIAN_POINT ( 'NONE',  ( -36.68005392025794009, -32.00140427513057517, -6.754974922286504757 ) ) ;
#379 = CARTESIAN_POINT ( 'NONE',  ( 2.886521338340684917, 1.601138781673192758E-19, 0.000000000000000000 ) ) ;
#380 = LINE ( 'NONE', #8542, #1299 ) ;
#381 = CARTESIAN_POINT ( 'NONE',  ( -33.35889894354067309, -7.999999999999996447, 124.0000000000000000 ) ) ;
#382 = DIRECTION ( 'NONE',  ( -0.000000000000000000, 0.000000000000000000, 1.000000000000000000 ) ) ;
#383 = CONICAL_SURFACE ( 'NONE', #2372, 1.649999999999998579, 1.029744258676653645 ) ;
#384 = CARTESIAN_POINT ( 'NONE',  ( -2.071067811865475505, -49.99999999999996447, -95.64999999999999147 ) ) ;
#385 = ORIENTED_EDGE ( 'NONE', *, *, #4770, .T. ) ;
#386 = CARTESIAN_POINT ( 'NONE',  ( -33.90612223281073057, -49.10140427513058370, 7.549504333439023718 ) ) ;
#387 = EDGE_LOOP ( 'NONE', ( #8592, #8016, #455, #3412 ) ) ;
#388 = CARTESIAN_POINT ( 'NONE',  ( -2.071067811865475061, -39.99999999999997158, -96.75000000000001421 ) ) ;
#389 = CARTESIAN_POINT ( 'NONE',  ( -4.999999999999998224, -44.99999999999997158, -97.29999999781504982 ) ) ;
#390 = PLANE ( 'NONE',  #4662 ) ;
#391 = DIRECTION ( 'NONE',  ( 0.000000000000000000, 0.000000000000000000, -1.000000000000000000 ) ) ;
#392 = FACE_OUTER_BOUND ( 'NONE', #2100, .T. ) ;
#393 = CARTESIAN_POINT ( 'NONE',  ( -4.999999999999998224, -42.92893218813449607, -98.25000000000000000 ) ) ;
#394 = DIRECTION ( 'NONE',  ( -1.000000000000000000, -0.000000000000000000, -0.000000000000000000 ) ) ;
#395 = EDGE_CURVE ( 'NONE', #6859, #7279, #4993, .T. ) ;
#396 = DIRECTION ( 'NONE',  ( 0.000000000000000000, 0.000000000000000000, -1.000000000000000000 ) ) ;
#397 = CARTESIAN_POINT ( 'NONE',  ( -20.13408869516454303, -43.04999999999999716, -1.562606840307982692 ) ) ;
#398 = ORIENTED_EDGE ( 'NONE', *, *, #4779, .F. ) ;
#399 = CARTESIAN_POINT ( 'NONE',  ( -28.49241082802385350, -31.44859572486944188, -9.874625247442173404 ) ) ;
#400 = CARTESIAN_POINT ( 'NONE',  ( -25.46513832392765408, -40.65000000000000568, 8.900167166472096270 ) ) ;
#401 = CARTESIAN_POINT ( 'NONE',  ( -23.64089511245930098, -35.75140427513057517, -6.280328284105564762 ) ) ;
#402 = CARTESIAN_POINT ( 'NONE',  ( -4.999999999999998224, -44.99999999999997158, -95.79999999999999716 ) ) ;
#403 = CARTESIAN_POINT ( 'NONE',  ( 33.05708889405230622, -41.03022111473440958, 12.12354317000652770 ) ) ;
#404 = CARTESIAN_POINT ( 'NONE',  ( -20.13408869516453947, -34.04999999999998295, -1.562606840307983136 ) ) ;
#405 = DIRECTION ( 'NONE',  ( 0.000000000000000000, -0.8660254037844390407, -0.4999999999999992784 ) ) ;
#406 = DIRECTION ( 'NONE',  ( 1.000000000000000000, 0.000000000000000000, 0.000000000000000000 ) ) ;
#407 = CARTESIAN_POINT ( 'NONE',  ( -4.566987299999998307, -44.99999999999997158, -96.24999999890751212 ) ) ;
#408 = CIRCLE ( 'NONE', #1969, 1.000000000000000888 ) ;
#409 = ORIENTED_EDGE ( 'NONE', *, *, #2203, .F. ) ;
#410 =( NAMED_UNIT ( * ) SI_UNIT ( $, .STERADIAN. ) SOLID_ANGLE_UNIT ( ) );
#411 = CARTESIAN_POINT ( 'NONE',  ( -37.98859631114233792, -51.84859572486944757, -4.007875659808334490 ) ) ;
#412 = CARTESIAN_POINT ( 'NONE',  ( -25.46513832392765408, -49.64999999999999147, 8.900167166472096270 ) ) ;
#413 = ADVANCED_FACE ( 'NONE', ( #392 ), #7895, .T. ) ;
#414 = ORIENTED_EDGE ( 'NONE', *, *, #7534, .T. ) ;
#415 = CARTESIAN_POINT ( 'NONE',  ( -21.12512167993187973, -39.35140427513057659, 4.584493831696868860 ) ) ;
#416 = CIRCLE ( 'NONE', #3111, 0.5000000000000001110 ) ;
#417 = CARTESIAN_POINT ( 'NONE',  ( -30.33426447602078113, -49.99999999999997868, 12.49999999999998046 ) ) ;
#418 = DIRECTION ( 'NONE',  ( 0.000000000000000000, 0.000000000000000000, 1.000000000000000000 ) ) ;
#419 = FACE_OUTER_BOUND ( 'NONE', #3879, .T. ) ;
#420 = CARTESIAN_POINT ( 'NONE',  ( -2.071067811865475061, -39.99999999999997158, -95.15000000000000568 ) ) ;
#421 = ORIENTED_EDGE ( 'NONE', *, *, #5864, .T. ) ;
#422 = CARTESIAN_POINT ( 'NONE',  ( -22.42644454439892598, -36.90000000000000568, -3.858919247786222861 ) ) ;
#423 = B_SPLINE_CURVE_WITH_KNOTS ( 'NONE', 3,
 ( #808, #6973, #5609, #147, #3632, #5471 ),
 .UNSPECIFIED., .F., .F.,
 ( 4, 2, 4 ),
 ( 0.1250000000000000000, 0.1875000000000000000, 0.2500000000000000000 ),
 .UNSPECIFIED. ) ;
#424 = ORIENTED_EDGE ( 'NONE', *, *, #7210, .T. ) ;
#425 = PRODUCT_DEFINITION_CONTEXT ( 'detailed design', #6216, 'design' ) ;
#426 = CARTESIAN_POINT ( 'NONE',  ( -3.061616997868382155E-16, -39.99999999999997158, -99.20000000000000284 ) ) ;
#427 = CARTESIAN_POINT ( 'NONE',  ( 2.528021161412670192, -49.35149720828152908, -99.99914980755436034 ) ) ;
#428 = EDGE_CURVE ( 'NONE', #5205, #1907, #5881, .T. ) ;
#429 = CYLINDRICAL_SURFACE ( 'NONE', #2354, 1.649999999999998579 ) ;
#430 = AXIS2_PLACEMENT_3D ( 'NONE', #3933, #522, #4634 ) ;
#431 = LINE ( 'NONE', #3098, #1438 ) ;
#432 = CARTESIAN_POINT ( 'NONE',  ( 4.000000000000003553, 0.000000000000000000, 0.000000000000000000 ) ) ;
#433 = DIRECTION ( 'NONE',  ( -0.000000000000000000, 1.000000000000000000, -0.000000000000000000 ) ) ;
#434 = CARTESIAN_POINT ( 'NONE',  ( 0.000000000000000000, -44.99999999999997158, -95.00000000000000000 ) ) ;
#435 = CARTESIAN_POINT ( 'NONE',  ( -21.09983283352783801, -46.34999999999999432, 4.534861676072186043 ) ) ;
#436 = ORIENTED_EDGE ( 'NONE', *, *, #4043, .T. ) ;
#437 = CARTESIAN_POINT ( 'NONE',  ( -38.81868038277247734, -45.54859572486944330, 1.453139578080855365 ) ) ;
#438 = CARTESIAN_POINT ( 'NONE',  ( -21.53543802021056663, -36.90000000000000568, -4.312909747525783821 ) ) ;
#439 = AXIS2_PLACEMENT_3D ( 'NONE', #6686, #1307, #1061 ) ;
#440 = CARTESIAN_POINT ( 'NONE',  ( -37.59760657776328685, -40.40140427513058086, 3.811716262761598362 ) ) ;
#441 = EDGE_CURVE ( 'NONE', #598, #864, #8558, .T. ) ;
#442 = CARTESIAN_POINT ( 'NONE',  ( 1.891708078845685481, -49.56698729999997255, -98.19999999890752918 ) ) ;
#443 = CARTESIAN_POINT ( 'NONE',  ( 33.76876201869192329, -41.69806059905381090, 11.92074493419279158 ) ) ;
#444 = CARTESIAN_POINT ( 'NONE',  ( -38.92545601287626056, -36.84859572486944046, -4.485229520447501450 ) ) ;
#445 = CARTESIAN_POINT ( 'NONE',  ( -31.48612741788231517, -36.30000000000000426, -9.383039235653804155 ) ) ;
#446 = DIRECTION ( 'NONE',  ( 1.000000000000000000, 0.000000000000000000, 0.000000000000000000 ) ) ;
#447 = CARTESIAN_POINT ( 'NONE',  ( -50.00000000000002842, -44.99999999999997158, 0.000000000000000000 ) ) ;
#448 = COLOUR_RGB ( '', 0.66274510, 0.83137255, 0.94901961) ;
#449 = CARTESIAN_POINT ( 'NONE',  ( 1.891708078845682595, -40.43301269999998482, -98.09999999890750644 ) ) ;
#450 = ORIENTED_EDGE ( 'NONE', *, *, #3020, .T. ) ;
#451 = LINE ( 'NONE', #2589, #1885 ) ;
#452 = CARTESIAN_POINT ( 'NONE',  ( -31.38201786482021305, -49.29859572486945041, -8.387063443159975762 ) ) ;
#453 = CARTESIAN_POINT ( 'NONE',  ( -21.12512167993187973, -33.35140427513057659, 4.584493831696868860 ) ) ;
#454 = AXIS2_PLACEMENT_3D ( 'NONE', #6879, #842, #8222 ) ;
#455 = ORIENTED_EDGE ( 'NONE', *, *, #8086, .F. ) ;
#456 = ORIENTED_EDGE ( 'NONE', *, *, #629, .F. ) ;
#457 = CARTESIAN_POINT ( 'NONE',  ( -21.51138689804841420, -35.90140427513058086, -4.265706762501151772 ) ) ;
#458 = CARTESIAN_POINT ( 'NONE',  ( -30.66228279038040228, -49.96682304584954437, 12.48662461771948529 ) ) ;
#459 = DIRECTION ( 'NONE',  ( -0.000000000000000000, -0.000000000000000000, 1.000000000000000000 ) ) ;
#460 = CARTESIAN_POINT ( 'NONE',  ( -30.00000000000002487, 0.000000000000000000, -29.65000000000000213 ) ) ;
#461 = DIRECTION ( 'NONE',  ( -0.000000000000000000, 1.000000000000000000, -0.000000000000000000 ) ) ;
#462 = CARTESIAN_POINT ( 'NONE',  ( -3.535533905932736864, -41.46446609406723383, -97.50000000000000000 ) ) ;
#463 = ORIENTED_EDGE ( 'NONE', *, *, #2478, .F. ) ;
#464 = CARTESIAN_POINT ( 'NONE',  ( -37.96330746473829976, -38.85000000000001563, -4.057507815433013754 ) ) ;
#465 = EDGE_CURVE ( 'NONE', #4613, #1975, #7431, .T. ) ;
#466 = AXIS2_PLACEMENT_3D ( 'NONE', #6133, #6787, #2038 ) ;
#467 = ORIENTED_EDGE ( 'NONE', *, *, #5580, .T. ) ;
#468 = CARTESIAN_POINT ( 'NONE',  ( -3.061616997868382155E-16, -39.99999999999997158, -97.60000000000000853 ) ) ;
#469 = CARTESIAN_POINT ( 'NONE',  ( -26.64110105645932336, 8.000000000000000000, -23.99999999999999289 ) ) ;
#470 = CARTESIAN_POINT ( 'NONE',  ( -24.02705286092866643, -33.50140427513058228, 6.047868141099968398 ) ) ;
#471 = CARTESIAN_POINT ( 'NONE',  ( -33.35889894354067309, 8.000000000000000000, 125.0000000000000000 ) ) ;
#472 = CARTESIAN_POINT ( 'NONE',  ( 4.999999999999998224, -44.99999999999997158, -96.89999999781505835 ) ) ;
#473 = CARTESIAN_POINT ( 'NONE',  ( -23.68028341417693738, -36.75000000000000711, -6.319716585823200283 ) ) ;
#474 = LINE ( 'NONE', #7771, #1262 ) ;
#475 = CARTESIAN_POINT ( 'NONE',  ( -37.06321265474346660, -47.25000000000000711, 7.063212654743582952 ) ) ;
#476 = DIRECTION ( 'NONE',  ( 0.000000000000000000, 0.000000000000000000, 1.000000000000000000 ) ) ;
#477 = ORIENTED_EDGE ( 'NONE', *, *, #3290, .F. ) ;
#478 = CARTESIAN_POINT ( 'NONE',  ( -26.18828373723858149, -46.59859572486944046, -7.597606577763319713 ) ) ;
#479 = CARTESIAN_POINT ( 'NONE',  ( -39.86591130483550671, -38.54999999999999716, 1.562606840307984468 ) ) ;
#480 = CARTESIAN_POINT ( 'NONE',  ( -33.90612223281073057, -40.10140427513057659, 7.549504333439023718 ) ) ;
#481 = VECTOR ( 'NONE', #6597, 1000.000000000000000 ) ;
#482 = CARTESIAN_POINT ( 'NONE',  ( -3.229347689422840784, -41.77065231057713390, -99.34999999890753486 ) ) ;
#483 = PLANE ( 'NONE',  #6432 ) ;
#484 = CARTESIAN_POINT ( 'NONE',  ( -21.55948914237271907, -40.89859572486943762, -4.360112732550413206 ) ) ;
#485 = CARTESIAN_POINT ( 'NONE',  ( -38.46456197978948666, -35.40000000000000568, 4.312909747525784709 ) ) ;
#486 = EDGE_CURVE ( 'NONE', #2955, #4083, #3727, .T. ) ;
#487 = CARTESIAN_POINT ( 'NONE',  ( -18.00000000000023093, 1.469576158976798506E-15, -45.00000000000000000 ) ) ;
#488 = CARTESIAN_POINT ( 'NONE',  ( -4.566987299999998307, -44.99999999999997158, -96.04999999890752349 ) ) ;
#489 = TOROIDAL_SURFACE ( 'NONE', #7690, 2.000000000000000000, 1.000000000000000000 ) ;
#490 =( LENGTH_UNIT ( ) NAMED_UNIT ( * ) SI_UNIT ( .MILLI., .METRE. ) );
#491 = ORIENTED_EDGE ( 'NONE', *, *, #6060, .T. ) ;
#492 = SURFACE_SIDE_STYLE ('',( #7789 ) ) ;
#493 = CARTESIAN_POINT ( 'NONE',  ( -34.26570676250101855, -33.09859572486943335, 8.488613101951703044 ) ) ;
#494 = CARTESIAN_POINT ( 'NONE',  ( -28.56619749409589204, -33.80140427513056522, 9.391326687552490782 ) ) ;
#495 = EDGE_CURVE ( 'NONE', #3168, #8538, #1819, .T. ) ;
#496 = AXIS2_PLACEMENT_3D ( 'NONE', #718, #6149, #4079 ) ;
#497 = ORIENTED_EDGE ( 'NONE', *, *, #3286, .F. ) ;
#498 = ORIENTED_EDGE ( 'NONE', *, *, #6490, .F. ) ;
#499 = CARTESIAN_POINT ( 'NONE',  ( -25.63988726744978663, -38.60140427513057659, -8.440510857627391061 ) ) ;
#500 = CARTESIAN_POINT ( 'NONE',  ( -34.82961390090871134, -46.30459253935130448, 11.52942094433410425 ) ) ;
#501 = CARTESIAN_POINT ( 'NONE',  ( 0.000000000000000000, 0.000000000000000000, 0.000000000000000000 ) ) ;
#502 = CARTESIAN_POINT ( 'NONE',  ( 4.999999999999998224, -44.99999999999997158, -97.00000000000000000 ) ) ;
#503 = CARTESIAN_POINT ( 'NONE',  ( -3.535533905932736864, -41.46446609406723383, -99.90000000000000568 ) ) ;
#504 = EDGE_CURVE ( 'NONE', #3192, #4124, #958, .T. ) ;
#505 = VERTEX_POINT ( 'NONE', #7187 ) ;
#506 = AXIS2_PLACEMENT_3D ( 'NONE', #7866, #2374, #8526 ) ;
#507 = CARTESIAN_POINT ( 'NONE',  ( -21.60464910494133406, -40.20000000000000995, 1.329692952841886155 ) ) ;
#508 = ADVANCED_FACE ( 'NONE', ( #3062, #1146 ), #5739, .F. ) ;
#509 = AXIS2_PLACEMENT_3D ( 'NONE', #6567, #6609, #5371 ) ;
#510 = ORIENTED_EDGE ( 'NONE', *, *, #7673, .F. ) ;
#511 = DIRECTION ( 'NONE',  ( 0.000000000000000000, 0.000000000000000000, 1.000000000000000000 ) ) ;
#512 = CARTESIAN_POINT ( 'NONE',  ( 2.071067811865474173, -39.99999999999997158, -97.64999999999999147 ) ) ;
#513 = CARTESIAN_POINT ( 'NONE',  ( -39.38303923565386100, -35.70000000000000995, -1.486127417882099788 ) ) ;
#514 = CARTESIAN_POINT ( 'NONE',  ( -4.961280561519337162, -44.31574741195442613, -99.99919817926395638 ) ) ;
#515 = EDGE_CURVE ( 'NONE', #71, #2692, #2215, .T. ) ;
#516 = CARTESIAN_POINT ( 'NONE',  ( -34.00787565980851213, -32.15140427513058086, -7.988596311142238449 ) ) ;
#517 = AXIS2_PLACEMENT_3D ( 'NONE', #552, #1736, #7060 ) ;
#518 = CARTESIAN_POINT ( 'NONE',  ( -41.99999999999996447, 48.00000000000002842, 20.35000000000000142 ) ) ;
#519 = CARTESIAN_POINT ( 'NONE',  ( -38.82739432537914581, -38.55000000000000426, 1.398121909749243663 ) ) ;
#520 = DIRECTION ( 'NONE',  ( 0.000000000000000000, 0.000000000000000000, 1.000000000000000000 ) ) ;
#521 = CARTESIAN_POINT ( 'NONE',  ( -21.53543802021056663, -48.90000000000000568, -4.312909747525783821 ) ) ;
#522 = DIRECTION ( 'NONE',  ( 0.000000000000000000, 1.000000000000000000, 0.000000000000000000 ) ) ;
#523 = ORIENTED_EDGE ( 'NONE', *, *, #1974, .F. ) ;
#524 = CARTESIAN_POINT ( 'NONE',  ( -37.54950433343896776, -48.39859572486944472, 3.906122232810848249 ) ) ;
#525 = CARTESIAN_POINT ( 'NONE',  ( -39.38303923565386100, -35.70000000000000995, -1.486127417882099788 ) ) ;
#526 = CARTESIAN_POINT ( 'NONE',  ( -35.97294713907137975, -35.00140427513057517, -6.047868141099968398 ) ) ;
#527 = CLOSED_SHELL ( 'NONE', ( #5613, #7239, #5879, #6349, #2268, #2193, #5062, #3908, #2590, #5355, #6240, #6891, #7681, #6961, #3590, #7937, #508, #6501, #1125, #2411, #1851, #6598, #8377, #3918, #1178, #796, #1378, #5792, #2216, #3557, #4936, #1316, #7178, #7893, #8060, #1449, #7304, #1330, #3411, #2383, #6115, #1171, #7572, #8073, #5454, #4555, #3146 ) ) ;
#528 = CARTESIAN_POINT ( 'NONE',  ( 4.999999999999998224, -42.92893218813449607, -96.15000000000000568 ) ) ;
#529 = CARTESIAN_POINT ( 'NONE',  ( 30.00000000000000000, -49.99999999999997158, -1.102182119232617753E-14 ) ) ;
#530 = CARTESIAN_POINT ( 'NONE',  ( -31.50758917197619979, -41.94859572486944188, 9.874625247442176956 ) ) ;
#531 = CARTESIAN_POINT ( 'NONE',  ( -20.61696076434619584, -43.20000000000000995, 1.486127417882100676 ) ) ;
#532 = PLANE ( 'NONE',  #3808 ) ;
#533 = ADVANCED_FACE ( 'NONE', ( #4459 ), #1022, .F. ) ;
#534 = CARTESIAN_POINT ( 'NONE',  ( 30.00000000000000000, 60.00000000000002842, -1.102182119232617753E-14 ) ) ;
#535 = CARTESIAN_POINT ( 'NONE',  ( 4.566987299999998307, -44.99999999999997158, -96.44999999890752918 ) ) ;
#536 =( NAMED_UNIT ( * ) SI_UNIT ( $, .STERADIAN. ) SOLID_ANGLE_UNIT ( ) );
#537 = ORIENTED_EDGE ( 'NONE', *, *, #6250, .F. ) ;
#538 = DIRECTION ( 'NONE',  ( 0.000000000000000000, 0.000000000000000000, -1.000000000000000000 ) ) ;
#539 = CARTESIAN_POINT ( 'NONE',  ( -21.59636165304264921, -47.19859572486943478, 1.277368040863740228 ) ) ;
#540 = CARTESIAN_POINT ( 'NONE',  ( -39.87462524744216807, -34.55140427513057233, 1.507589171976367215 ) ) ;
#541 = ORIENTED_EDGE ( 'NONE', *, *, #2221, .F. ) ;
#542 = ORIENTED_EDGE ( 'NONE', *, *, #7814, .F. ) ;
#543 = CARTESIAN_POINT ( 'NONE',  ( -28.38237549136062654, -44.45140427513058512, -9.857197362228843573 ) ) ;
#544 = CARTESIAN_POINT ( 'NONE',  ( -39.99999999999999289, 1.224646799147353059E-15, 60.00000000000002842 ) ) ;
#545 = CARTESIAN_POINT ( 'NONE',  ( -44.14999999999995595, 22.00000000000000000, 60.00000000000002842 ) ) ;
#546 = TOROIDAL_SURFACE ( 'NONE', #3100, 11.32499999999999929, 1.324999999999999956 ) ;
#547 = CARTESIAN_POINT ( 'NONE',  ( 3.535533905932736420, -41.46446609406723383, -95.99999999781503845 ) ) ;
#548 = CARTESIAN_POINT ( 'NONE',  ( 33.76617411639087152, -48.30471456237972205, 11.92153802757354342 ) ) ;
#549 = CARTESIAN_POINT ( 'NONE',  ( -50.00000000000002842, -30.00000000000000000, 60.00000000000002842 ) ) ;
#550 = EDGE_LOOP ( 'NONE', ( #7307, #8387, #6188 ) ) ;
#551 = CARTESIAN_POINT ( 'NONE',  ( -38.39535089505872634, -44.70000000000000284, -1.329692952841885267 ) ) ;
#552 = CARTESIAN_POINT ( 'NONE',  ( 42.00000000000000711, 21.99999999999992184, 60.00000000000002842 ) ) ;
#553 = CARTESIAN_POINT ( 'NONE',  ( -4.566987299999998307, -43.10829192115428299, -95.49999999890754054 ) ) ;
#554 = CARTESIAN_POINT ( 'NONE',  ( 4.999999999999998224, -44.99999999999997158, -97.69999999781505551 ) ) ;
#555 = CARTESIAN_POINT ( 'NONE',  ( -22.93678734525658314, -39.74999999999999289, -7.063212654743582952 ) ) ;
#556 = B_SPLINE_CURVE_WITH_KNOTS ( 'NONE', 3,
 ( #4547, #3887, #5995, #8125, #5416, #2084, #2749, #4769, #1411, #7454, #4108, #44, #6786, #749, #6087, #3810, #3729, #1657, #2452, #328 ),
 .UNSPECIFIED., .F., .F.,
 ( 4, 2, 2, 2, 2, 2, 2, 2, 2, 4 ),
 ( 2.088883680402604765E-17, 0.0009878455431464048045, 0.001975691086292788792, 0.002963536629439172780, 0.003951382172585556768, 0.004939227715731940756, 0.005927073258878324744, 0.006420996030451506763, 0.006914918802024689649, 0.007902764345171071902 ),
 .UNSPECIFIED. ) ;
#557 = CARTESIAN_POINT ( 'NONE',  ( -3.229347689422839451, -48.22934768942280925, -99.14999999890753202 ) ) ;
#558 = CARTESIAN_POINT ( 'NONE',  ( -2.227513643315880643, -40.48620403085396902, -99.99969435636208459 ) ) ;
#559 = CARTESIAN_POINT ( 'NONE',  ( -37.93801861833426159, -37.85140427513057659, -4.107139971057695682 ) ) ;
#560 = AXIS2_PLACEMENT_3D ( 'NONE', #4014, #4102, #4307 ) ;
#561 = CARTESIAN_POINT ( 'NONE',  ( 3.535533905932737309, -48.53553390593270933, -97.09300000002185982 ) ) ;
#562 = CARTESIAN_POINT ( 'NONE',  ( -34.05750781543319050, -39.14999999999999858, -7.963307464738194952 ) ) ;
#563 = CARTESIAN_POINT ( 'NONE',  ( -42.00000000000002132, 0.000000000000000000, -29.65000000000000213 ) ) ;
#564 =( GEOMETRIC_REPRESENTATION_CONTEXT ( 3 ) GLOBAL_UNCERTAINTY_ASSIGNED_CONTEXT ( ( #7738 ) ) GLOBAL_UNIT_ASSIGNED_CONTEXT ( ( #896, #4163, #2803 ) ) REPRESENTATION_CONTEXT ( 'NONE', 'WORKASPACE' ) );
#565 = CARTESIAN_POINT ( 'NONE',  ( -39.86591130483550671, -50.55000000000001137, 1.562606840307984690 ) ) ;
#566 = DIRECTION ( 'NONE',  ( 0.000000000000000000, 0.000000000000000000, 1.000000000000000000 ) ) ;
#567 = EDGE_LOOP ( 'NONE', ( #498, #2058, #5139, #6935, #113, #2462 ) ) ;
#568 = CARTESIAN_POINT ( 'NONE',  ( 33.61000000000001364, 0.000000000000000000, 0.000000000000000000 ) ) ;
#569 = CARTESIAN_POINT ( 'NONE',  ( -36.71751442127229836, -39.00000000000000711, -6.717514421272142044 ) ) ;
#570 = CARTESIAN_POINT ( 'NONE',  ( -34.00787565980851213, -38.15140427513058086, -7.988596311142238449 ) ) ;
#571 = AXIS2_PLACEMENT_3D ( 'NONE', #8605, #6041, #8689 ) ;
#572 = PLANE ( 'NONE',  #1496 ) ;
#573 = CARTESIAN_POINT ( 'NONE',  ( -25.41550616830297571, -32.64859572486943762, 8.874878320068054549 ) ) ;
#574 = CARTESIAN_POINT ( 'NONE',  ( -31.50758917197619979, -32.94859572486944188, 9.874625247442176956 ) ) ;
#575 = AXIS2_PLACEMENT_3D ( 'NONE', #8671, #6590, #5266 ) ;
#576 = CARTESIAN_POINT ( 'NONE',  ( 42.00000000000000711, -21.99999999999992184, 80.00000000000002842 ) ) ;
#577 = DIRECTION ( 'NONE',  ( -1.000000000000000000, -0.000000000000000000, -0.000000000000000000 ) ) ;
#578 = CARTESIAN_POINT ( 'NONE',  ( 4.566987300000000083, -46.89170807884565306, -99.09999999890752065 ) ) ;
#579 = AXIS2_PLACEMENT_3D ( 'NONE', #3617, #8335, #2961 ) ;
#580 = VERTEX_POINT ( 'NONE', #7145 ) ;
#581 = CARTESIAN_POINT ( 'NONE',  ( -4.999999999999998224, -44.99999999999997158, -95.00000000000000000 ) ) ;
#582 = CARTESIAN_POINT ( 'NONE',  ( -36.01040764008574513, -48.00000000000000711, -6.010407640085605685 ) ) ;
#583 = CARTESIAN_POINT ( 'NONE',  ( -23.24502507771338600, -32.49859572486943904, 6.680053920257780220 ) ) ;
#584 = CARTESIAN_POINT ( 'NONE',  ( -20.62524821624488069, -36.20140427513057091, 1.538452329860250378 ) ) ;
#585 = ORIENTED_EDGE ( 'NONE', *, *, #701, .F. ) ;
#586 = ORIENTED_EDGE ( 'NONE', *, *, #2638, .T. ) ;
#587 = CIRCLE ( 'NONE', #335, 2.200000000000001066 ) ;
#588 = CARTESIAN_POINT ( 'NONE',  ( -20.12537475255788522, -42.05140427513057944, -1.507589171976365439 ) ) ;
#589 = MECHANICAL_DESIGN_GEOMETRIC_PRESENTATION_REPRESENTATION (  '', ( #39 ), #3149 ) ;
#590 =( LENGTH_UNIT ( ) NAMED_UNIT ( * ) SI_UNIT ( .MILLI., .METRE. ) );
#591 = CARTESIAN_POINT ( 'NONE',  ( 4.999999999999998224, -44.99999999999997158, -98.49999999781503845 ) ) ;
#592 = CARTESIAN_POINT ( 'NONE',  ( 3.535533905932737309, -48.53553390593270933, -98.59999999781504698 ) ) ;
#593 = CARTESIAN_POINT ( 'NONE',  ( 4.999999999999998224, -44.99999999999997158, -95.00000000000000000 ) ) ;
#594 = CARTESIAN_POINT ( 'NONE',  ( 3.535533905932736420, -41.46446609406723383, -99.29999999999999716 ) ) ;
#595 = EDGE_LOOP ( 'NONE', ( #4745, #2458, #2730, #1335 ) ) ;
#596 = CARTESIAN_POINT ( 'NONE',  ( -31.39812190974910422, -43.95000000000000284, 8.827394325379140483 ) ) ;
#597 = VECTOR ( 'NONE', #1210, 1000.000000000000000 ) ;
#598 = VERTEX_POINT ( 'NONE', #8559 ) ;
#599 = CARTESIAN_POINT ( 'NONE',  ( -3.229347689422840784, -41.77065231057713390, -98.74999999890751212 ) ) ;
#600 = CARTESIAN_POINT ( 'NONE',  ( -4.999999999999998224, -45.95670858091268940, -95.67690300950226856 ) ) ;
#601 = CARTESIAN_POINT ( 'NONE',  ( -31.48612741788231517, -42.30000000000000426, -9.383039235653804155 ) ) ;
#602 = CARTESIAN_POINT ( 'NONE',  ( 4.566987300000000083, -46.89170807884565306, -97.29999999890750928 ) ) ;
#603 = CARTESIAN_POINT ( 'NONE',  ( -4.111674810624561971, -47.85923343201969260, -99.99917207927896357 ) ) ;
#604 = CARTESIAN_POINT ( 'NONE',  ( -22.06198138166579170, -36.35140427513057659, 4.107139971057695682 ) ) ;
#605 = VECTOR ( 'NONE', #8413, 1000.000000000000000 ) ;
#606 = ADVANCED_FACE ( 'NONE', ( #2522, #3714 ), #3797, .T. ) ;
#607 = CARTESIAN_POINT ( 'NONE',  ( -2.071067811865475061, -39.99999999999997158, -97.54300000002184845 ) ) ;
#608 = UNCERTAINTY_MEASURE_WITH_UNIT (LENGTH_MEASURE( 1.000000000000000082E-05 ), #1837, 'distance_accuracy_value', 'NONE');
#609 = CARTESIAN_POINT ( 'NONE',  ( -36.31971658582311591, -38.25000000000000711, 6.319716585823200283 ) ) ;
#610 = CARTESIAN_POINT ( 'NONE',  ( 34.00000000000000000, 0.000000000000000000, 0.000000000000000000 ) ) ;
#611 = CARTESIAN_POINT ( 'NONE',  ( -28.43739315969223824, -48.45000000000000284, -9.865911304835512041 ) ) ;
#612 = EDGE_CURVE ( 'NONE', #7038, #4661, #5452, .T. ) ;
#613 =( NAMED_UNIT ( * ) PLANE_ANGLE_UNIT ( ) SI_UNIT ( $, .RADIAN. ) );
#614 = EDGE_LOOP ( 'NONE', ( #6274, #1845, #5331, #7137 ) ) ;
#615 = CARTESIAN_POINT ( 'NONE',  ( -26.64110105645932336, 9.000000000000001776, 125.0000000000000000 ) ) ;
#616 = CARTESIAN_POINT ( 'NONE',  ( -31.48612741788231517, -42.30000000000000426, -9.383039235653804155 ) ) ;
#617 = CARTESIAN_POINT ( 'NONE',  ( -26.09387776718931917, -44.60140427513058370, -7.549504333439021941 ) ) ;
#618 = LINE ( 'NONE', #2581, #6843 ) ;
#619 = ADVANCED_FACE ( 'NONE', ( #8516 ), #6422, .T. ) ;
#620 = DIRECTION ( 'NONE',  ( -0.000000000000000000, 1.000000000000000000, -0.000000000000000000 ) ) ;
#621 = CARTESIAN_POINT ( 'NONE',  ( -34.58449383169706692, -40.14859572486943762, -8.874878320068054549 ) ) ;
#622 = CARTESIAN_POINT ( 'NONE',  ( 4.999999999999998224, -44.99999999999997158, -99.29999999781504982 ) ) ;
#623 = DIRECTION ( 'NONE',  ( -1.000000000000000000, -0.000000000000000000, -0.000000000000000000 ) ) ;
#624 = CARTESIAN_POINT ( 'NONE',  ( -4.566987299999997418, -46.89170807884566727, -99.39999999890751781 ) ) ;
#625 = EDGE_LOOP ( 'NONE', ( #5700, #4753, #2629, #4443 ) ) ;
#626 = CARTESIAN_POINT ( 'NONE',  ( -50.00000000000002842, -44.99999999999997158, 2.099999999999997868 ) ) ;
#627 = AXIS2_PLACEMENT_3D ( 'NONE', #1489, #300, #3700 ) ;
#628 = CARTESIAN_POINT ( 'NONE',  ( -25.94249218456686279, -49.64999999999999147, 7.963307464738195840 ) ) ;
#629 = EDGE_CURVE ( 'NONE', #4891, #8357, #1533, .T. ) ;
#630 = CARTESIAN_POINT ( 'NONE',  ( -39.39132668755255651, -39.69859572486944188, -1.433802505903950308 ) ) ;
#631 = CARTESIAN_POINT ( 'NONE',  ( -25.63988726744978663, -44.60140427513058370, -8.440510857627391061 ) ) ;
#632 = EDGE_LOOP ( 'NONE', ( #5483, #7666, #5670, #7686 ) ) ;
#633 =( REPRESENTATION_RELATIONSHIP ('NONE','NONE', #2265, #7097 ) REPRESENTATION_RELATIONSHIP_WITH_TRANSFORMATION ( #5735 )SHAPE_REPRESENTATION_RELATIONSHIP( ) );
#634 = EDGE_LOOP ( 'NONE', ( #2546, #1880, #6420, #7835 ) ) ;
#635 = CARTESIAN_POINT ( 'NONE',  ( -37.10260095646111012, -46.25140427513058228, 7.023824353025939438 ) ) ;
#636 = EDGE_CURVE ( 'NONE', #5681, #7609, #5596, .T. ) ;
#637 = FILL_AREA_STYLE_COLOUR ( '', #448 ) ;
#638 = LINE ( 'NONE', #4044, #1797 ) ;
#639 = CARTESIAN_POINT ( 'NONE',  ( 1.891708078845682595, -40.43301269999998482, -95.69999999890751496 ) ) ;
#640 = CARTESIAN_POINT ( 'NONE',  ( -3.535533905932735532, -48.53553390593270933, -96.50000000000000000 ) ) ;
#641 = CARTESIAN_POINT ( 'NONE',  ( -2.071067811865475061, -39.99999999999997158, -99.94999999999998863 ) ) ;
#642 = ORIENTED_EDGE ( 'NONE', *, *, #4452, .F. ) ;
#643 = CARTESIAN_POINT ( 'NONE',  ( -31.39812190974910422, -46.94999999999998863, 8.827394325379140483 ) ) ;
#644 = DIRECTION ( 'NONE',  ( 1.000000000000000000, 0.000000000000000000, 0.000000000000000000 ) ) ;
#645 = CIRCLE ( 'NONE', #5579, 1.649999999999998579 ) ;
#646 = EDGE_LOOP ( 'NONE', ( #7860, #1088, #1174 ) ) ;
#647 = CARTESIAN_POINT ( 'NONE',  ( -1.891708078845683705, -49.56698729999997255, -99.29999999890752349 ) ) ;
#648 = CARTESIAN_POINT ( 'NONE',  ( 2.071067811865477282, -49.99999999999996447, -99.54999999999998295 ) ) ;
#649 = CARTESIAN_POINT ( 'NONE',  ( -20.13408869516453947, -40.05000000000001137, -1.562606840307983136 ) ) ;
#650 = CARTESIAN_POINT ( 'NONE',  ( 4.566987299999998307, -44.99999999999997158, -98.84999999890753486 ) ) ;
#651 = CARTESIAN_POINT ( 'NONE',  ( -31.74999999999995737, 4.286263797015736595E-16, -3.500000000000000000 ) ) ;
#652 = CARTESIAN_POINT ( 'NONE',  ( -23.64089511245930098, -32.75140427513057517, -6.280328284105564762 ) ) ;
#653 = AXIS2_PLACEMENT_3D ( 'NONE', #4860, #1588, #6305 ) ;
#654 = AXIS2_PLACEMENT_3D ( 'NONE', #7280, #754, #5374 ) ;
#655 = CIRCLE ( 'NONE', #1387, 2.149999999999985256 ) ;
#656 = CARTESIAN_POINT ( 'NONE',  ( 4.999999999999998224, -42.92893218813448897, -97.74300000002186550 ) ) ;
#657 = CARTESIAN_POINT ( 'NONE',  ( -26.14108075221394856, -39.60000000000000853, -7.573555455601170827 ) ) ;
#658 = CARTESIAN_POINT ( 'NONE',  ( -17.99999999999998579, 1.469576158976828483E-15, -29.65000000000000213 ) ) ;
#659 = DIRECTION ( 'NONE',  ( -0.000000000000000000, -0.000000000000000000, -1.000000000000000000 ) ) ;
#660 = CARTESIAN_POINT ( 'NONE',  ( -41.99999999999996447, 84.00000000000002842, 22.00000000000000000 ) ) ;
#661 = ORIENTED_EDGE ( 'NONE', *, *, #5691, .T. ) ;
#662 = DIRECTION ( 'NONE',  ( 1.000000000000000000, 0.000000000000000000, 0.000000000000000000 ) ) ;
#663 = AXIS2_PLACEMENT_3D ( 'NONE', #432, #3150, #5826 ) ;
#664 = CARTESIAN_POINT ( 'NONE',  ( -20.61696076434619584, -43.20000000000000995, 1.486127417882100676 ) ) ;
#665 = CARTESIAN_POINT ( 'NONE',  ( -31.27736804086391942, -44.30140427513057944, -8.403638346957361449 ) ) ;
#666 = ADVANCED_FACE ( 'NONE', ( #7216 ), #4530, .T. ) ;
#667 = FACE_BOUND ( 'NONE', #7929, .T. ) ;
#668 = DIRECTION ( 'NONE',  ( 0.000000000000000000, 0.000000000000000000, -1.000000000000000000 ) ) ;
#669 = CARTESIAN_POINT ( 'NONE',  ( -25.41550616830297571, -44.64859572486944472, 8.874878320068054549 ) ) ;
#670 = DIRECTION ( 'NONE',  ( -0.000000000000000000, -0.000000000000000000, 1.000000000000000000 ) ) ;
#671 = DIRECTION ( 'NONE',  ( -0.000000000000000000, 1.000000000000000000, -0.000000000000000000 ) ) ;
#672 = CARTESIAN_POINT ( 'NONE',  ( 8.389419568037416259E-16, -49.56698729999997255, -100.0499999989075093 ) ) ;
#673 = ORIENTED_EDGE ( 'NONE', *, *, #4128, .F. ) ;
#674 = LINE ( 'NONE', #8046, #3482 ) ;
#675 = CARTESIAN_POINT ( 'NONE',  ( -23.98959235991431171, -49.50000000000000711, 6.010407640085604797 ) ) ;
#676 =( BOUNDED_CURVE ( )  B_SPLINE_CURVE ( 2, ( #4826, #8092, #6187, #2185, #3465, #6930, #895, #2098, #6231, #6802, #7424, #2049, #809, #6886, #192, #4873, #4781, #4738, #1380, #7548, #1425, #4076, #6753, #715, #3422, #4120, #1469, #6146, #148, #57, #105, #2802, #5472, #850, #4162, #6842, #1512, #2893, #2232, #4911, #7635, #3067, #8480, #8441, #359, #4291, #232, #6445, #7018, #7683, #2935, #2363, #7817, #5745, #5610, #5785, #1027, #2405, #1070, #2445, #5698, #1783, #5083, #8311, #5126, #5654, #3721, #2275, #7772, #4955, #6315, #6974, #7731, #1741, #939, #3633, #5040, #8400, #1691, #6403, #1110, #4382, #4463, #3761, #4426, #6273, #7109, #397, #3104, #7066, #277, #3677, #1600, #6357, #2979, #320, #8355, #2320, #4998, #3026, #7149, #1646, #4338, #980, #8650, #5956, #8688, #1865, #3232, #435, #6527, #2615, #5283, #7322, #7943, #475, #7857, #3153, #5203, #7989, #7898, #2525, #5330, #611, #6655, #8604, #521, #1823, #5829, #1193, #3278, #1992, #8519, #2485, #1277, #4593, #3802, #565, #3190, #1150, #3324 ),
 .UNSPECIFIED., .F., .T. ) 
 B_SPLINE_CURVE_WITH_KNOTS ( ( 3, 2, 2, 2, 2, 2, 2, 2, 2, 2, 2, 2, 2, 2, 2, 2, 2, 2, 2, 2, 2, 2, 2, 2, 2, 2, 2, 2, 2, 2, 2, 2, 2, 2, 2, 2, 2, 2, 2, 2, 2, 2, 2, 2, 2, 2, 2, 2, 2, 2, 2, 2, 2, 2, 2, 2, 2, 2, 2, 2, 2, 2, 2, 2, 2, 2, 2, 2, 2, 2, 3 ),
 ( 0.000000000000000000, 0.01428571428571428527, 0.02857142857142857054, 0.04285714285714285754, 0.05714285714285714107, 0.07142857142857142461, 0.08571428571428571508, 0.1000000000000000056, 0.1142857142857142821, 0.1285714285714285587, 0.1428571428571428492, 0.1571428571428571397, 0.1714285714285714302, 0.1857142857142857206, 0.2000000000000000111, 0.2142857142857142738, 0.2285714285714285643, 0.2428571428571428548, 0.2571428571428571175, 0.2714285714285714080, 0.2857142857142856984, 0.2999999999999999889, 0.3142857142857142794, 0.3285714285714285698, 0.3428571428571428603, 0.3571428571428571508, 0.3714285714285714413, 0.3857142857142857317, 0.4000000000000000222, 0.4142857142857143127, 0.4285714285714285476, 0.4428571428571428381, 0.4571428571428571286, 0.4714285714285714191, 0.4857142857142857095, 0.5000000000000000000, 0.5142857142857142350, 0.5285714285714285809, 0.5428571428571428159, 0.5571428571428571619, 0.5714285714285713969, 0.5857142857142857428, 0.5999999999999999778, 0.6142857142857143238, 0.6285714285714285587, 0.6428571428571429047, 0.6571428571428571397, 0.6714285714285713746, 0.6857142857142857206, 0.6999999999999999556, 0.7142857142857143016, 0.7285714285714285365, 0.7428571428571428825, 0.7571428571428571175, 0.7714285714285714635, 0.7857142857142856984, 0.8000000000000000444, 0.8142857142857142794, 0.8285714285714286254, 0.8428571428571428603, 0.8571428571428570953, 0.8714285714285714413, 0.8857142857142856762, 0.9000000000000000222, 0.9142857142857142572, 0.9285714285714286031, 0.9428571428571428381, 0.9571428571428571841, 0.9714285714285714191, 0.9857142857142857650, 1.000000000000000000 ),
 .UNSPECIFIED. ) 
 CURVE ( )  GEOMETRIC_REPRESENTATION_ITEM ( )  RATIONAL_B_SPLINE_CURVE ( ( 1.000000000000000000, 0.9510565162951535312, 1.000000000000000000, 0.9510565162951535312, 1.000000000000000000, 0.9510565162951535312, 1.000000000000000000, 0.9510565162951535312, 1.000000000000000000, 0.9510565162951535312, 1.000000000000000000, 0.9510565162951535312, 1.000000000000000000, 0.9510565162951535312, 1.000000000000000000, 0.9510565162951535312, 1.000000000000000000, 0.9510565162951535312, 1.000000000000000000, 0.9510565162951535312, 1.000000000000000000, 0.9510565162951535312, 1.000000000000000000, 0.9510565162951535312, 1.000000000000000000, 0.9510565162951535312, 1.000000000000000000, 0.9510565162951535312, 1.000000000000000000, 0.9510565162951535312, 1.000000000000000000, 0.9510565162951535312, 1.000000000000000000, 0.9510565162951535312, 1.000000000000000000, 0.9510565162951535312, 1.000000000000000000, 0.9510565162951535312, 1.000000000000000000, 0.9510565162951535312, 1.000000000000000000, 0.9510565162951535312, 1.000000000000000000, 0.9510565162951535312, 1.000000000000000000, 0.9510565162951535312, 1.000000000000000000, 0.9510565162951535312, 1.000000000000000000, 0.9510565162951535312, 1.000000000000000000, 0.9510565162951535312, 1.000000000000000000, 0.9510565162951535312, 1.000000000000000000, 0.9510565162951535312, 1.000000000000000000, 0.9510565162951535312, 1.000000000000000000, 0.9510565162951535312, 1.000000000000000000, 0.9510565162951535312, 1.000000000000000000, 0.9510565162951535312, 1.000000000000000000, 0.9510565162951535312, 1.000000000000000000, 0.9510565162951535312, 1.000000000000000000, 0.9510565162951535312, 1.000000000000000000, 0.9510565162951535312, 1.000000000000000000, 0.9510565162951535312, 1.000000000000000000, 0.9510565162951535312, 1.000000000000000000, 0.9510565162951535312, 1.000000000000000000, 0.9510565162951535312, 1.000000000000000000, 0.9510565162951535312, 1.000000000000000000, 0.9510565162951535312, 1.000000000000000000, 0.9510565162951535312, 1.000000000000000000, 0.9510565162951535312, 1.000000000000000000, 0.9510565162951535312, 1.000000000000000000, 0.9510565162951535312, 1.000000000000000000, 0.9510565162951535312, 1.000000000000000000, 0.9510565162951535312, 1.000000000000000000, 0.9510565162951535312, 1.000000000000000000, 0.9510565162951535312, 1.000000000000000000, 0.9510565162951535312, 1.000000000000000000, 0.9510565162951535312, 1.000000000000000000, 0.9510565162951535312, 1.000000000000000000, 0.9510565162951535312, 1.000000000000000000, 0.9510565162951535312, 1.000000000000000000, 0.9510565162951535312, 1.000000000000000000, 0.9510565162951535312, 1.000000000000000000, 0.9510565162951535312, 1.000000000000000000, 0.9510565162951535312, 1.000000000000000000, 0.9510565162951535312, 1.000000000000000000, 0.9510565162951535312, 1.000000000000000000, 0.9510565162951535312, 1.000000000000000000, 0.9510565162951535312, 1.000000000000000000, 0.9510565162951535312, 1.000000000000000000, 0.9510565162951535312, 1.000000000000000000, 0.9510565162951535312, 1.000000000000000000, 0.9510565162951535312, 1.000000000000000000, 0.9510565162951535312, 1.000000000000000000, 0.9510565162951535312, 1.000000000000000000, 0.9510565162951535312, 1.000000000000000000 ) ) 
 REPRESENTATION_ITEM ( '' )  );
#677 = CARTESIAN_POINT ( 'NONE',  ( -36.75497492228666374, -39.99859572486943904, -6.680053920257780220 ) ) ;
#678 = CARTESIAN_POINT ( 'NONE',  ( -28.38237549136062654, -44.45140427513058512, -9.857197362228843573 ) ) ;
#679 = CLOSED_SHELL ( 'NONE', ( #7354, #6229, #8350, #1433, #4093, #6520, #7720, #1560, #7628, #4521, #4016, #3800, #5743, #3822, #7621, #4055, #7669, #4185, #6558, #1536, #3196, #3679, #1549, #5972, #76, #87, #7313, #7419, #7801, #4973, #8008, #2481, #4022, #3615, #4856, #2349, #5957, #8496, #3760, #533, #2845, #7262 ) ) ;
#680 = ORIENTED_EDGE ( 'NONE', *, *, #275, .T. ) ;
#681 = ORIENTED_EDGE ( 'NONE', *, *, #1766, .F. ) ;
#682 = CARTESIAN_POINT ( 'NONE',  ( -20.12537475255788522, -45.05140427513057944, -1.507589171976365439 ) ) ;
#683 = PRESENTATION_STYLE_ASSIGNMENT (( #2596 ) ) ;
#684 = CARTESIAN_POINT ( 'NONE',  ( 29.99999999999997158, 1.102182119232617753E-14, 80.00000000000002842 ) ) ;
#685 = CARTESIAN_POINT ( 'NONE',  ( -4.566987299999998307, -44.99999999999997158, -95.44999999890751496 ) ) ;
#686 = CARTESIAN_POINT ( 'NONE',  ( 32.51701891408353617, -49.33233869400790184, 12.24706002614420264 ) ) ;
#687 = CARTESIAN_POINT ( 'NONE',  ( 5.000000000000000000, -47.07106781186545419, -99.45000000000000284 ) ) ;
#688 = ORIENTED_EDGE ( 'NONE', *, *, #7144, .T. ) ;
#689 = EDGE_CURVE ( 'NONE', #4311, #8113, #1014, .T. ) ;
#690 = CARTESIAN_POINT ( 'NONE',  ( -23.71967171589458445, -34.74859572486943904, -6.359104887540838469 ) ) ;
#691 = CARTESIAN_POINT ( 'NONE',  ( -23.28248557872775137, -34.50000000000000000, 6.717514421272141156 ) ) ;
#692 = ORIENTED_EDGE ( 'NONE', *, *, #3230, .T. ) ;
#693 = CARTESIAN_POINT ( 'NONE',  ( 4.566987300000000083, -46.89170807884564596, -97.49999999890752633 ) ) ;
#694 = CARTESIAN_POINT ( 'NONE',  ( 4.999999999999998224, -42.92893218813448897, -99.35000000000000853 ) ) ;
#695 = CARTESIAN_POINT ( 'NONE',  ( -37.06321265474346660, -44.25000000000000000, 7.063212654743582952 ) ) ;
#696 = CARTESIAN_POINT ( 'NONE',  ( -2.796473189345805913E-16, -40.43301269999997061, -97.04999999890752349 ) ) ;
#697 = DIRECTION ( 'NONE',  ( -1.000000000000000000, 0.000000000000000000, 0.000000000000000000 ) ) ;
#698 = CARTESIAN_POINT ( 'NONE',  ( -35.97294713907137975, -41.00140427513057517, -6.047868141099968398 ) ) ;
#699 = CONICAL_SURFACE ( 'NONE', #7040, 12.49999999999997335, 1.029744258676651869 ) ;
#700 = CARTESIAN_POINT ( 'NONE',  ( -3.061616997868382155E-16, -39.99999999999997158, -95.99300000002185129 ) ) ;
#701 = EDGE_CURVE ( 'NONE', #2848, #7832, #7939, .T. ) ;
#702 = CARTESIAN_POINT ( 'NONE',  ( -33.85891924778610473, -44.10000000000000853, 7.573555455601171715 ) ) ;
#703 = LINE ( 'NONE', #3322, #4754 ) ;
#704 = LINE ( 'NONE', #2703, #2722 ) ;
#705 = ITEM_DEFINED_TRANSFORMATION ( 'NONE', 'NONE', #5802,  #2554 ) ;
#706 = AXIS2_PLACEMENT_3D ( 'NONE', #5991, #697, #8325 ) ;
#707 = ORIENTED_EDGE ( 'NONE', *, *, #8464, .T. ) ;
#708 = DIRECTION ( 'NONE',  ( 1.049727191138618079E-16, 0.5150380749100549327, -0.8571673007021118895 ) ) ;
#709 = CARTESIAN_POINT ( 'NONE',  ( -20.13408869516453947, -49.04999999999999716, -1.562606840307983136 ) ) ;
#710 = CARTESIAN_POINT ( 'NONE',  ( -26.09387776718931917, -47.60140427513058370, -7.549504333439021941 ) ) ;
#711 = CARTESIAN_POINT ( 'NONE',  ( -41.99999999999996447, 47.00857997860455129, -22.00000000000000000 ) ) ;
#712 = DIRECTION ( 'NONE',  ( 0.000000000000000000, 0.000000000000000000, 1.000000000000000000 ) ) ;
#713 = CARTESIAN_POINT ( 'NONE',  ( -39.85719736222883824, -51.54859572486944330, 1.617624508639602388 ) ) ;
#714 = CARTESIAN_POINT ( 'NONE',  ( -40.00000000000002842, 1.224646799147353059E-15, -40.35000000000000142 ) ) ;
#715 = CARTESIAN_POINT ( 'NONE',  ( -28.43739315969223824, -33.45000000000000995, -9.865911304835512041 ) ) ;
#716 = PRESENTATION_STYLE_ASSIGNMENT (( #3549 ) ) ;
#717 = ORIENTED_EDGE ( 'NONE', *, *, #3971, .F. ) ;
#718 = CARTESIAN_POINT ( 'NONE',  ( -36.36396103067902175, -51.00000000000000711, -6.363961030678874309 ) ) ;
#719 = CARTESIAN_POINT ( 'NONE',  ( -36.31971658582311591, -50.24999999999998579, 6.319716585823199395 ) ) ;
#720 = CARTESIAN_POINT ( 'NONE',  ( -21.07454398712378918, -38.34859572486944046, 4.485229520447505003 ) ) ;
#721 = CARTESIAN_POINT ( 'NONE',  ( -38.87487832006816291, -37.85140427513057659, -4.584493831696867971 ) ) ;
#722 = STYLED_ITEM ( 'NONE', ( #1742 ), #4644 ) ;
#723 = EDGE_CURVE ( 'NONE', #4083, #876, #2542, .T. ) ;
#724 = VERTEX_POINT ( 'NONE', #2388 ) ;
#725 = ORIENTED_EDGE ( 'NONE', *, *, #7163, .T. ) ;
#726 = CARTESIAN_POINT ( 'NONE',  ( -38.87487832006816291, -43.85140427513058370, -4.584493831696867971 ) ) ;
#727 =( LENGTH_UNIT ( ) NAMED_UNIT ( * ) SI_UNIT ( .MILLI., .METRE. ) );
#728 = DIRECTION ( 'NONE',  ( 1.049727191138617093E-16, 0.5150380749100563760, -0.8571673007021110013 ) ) ;
#729 = CARTESIAN_POINT ( 'NONE',  ( -4.999999999999998224, -44.99999999999997158, -100.4999999978150385 ) ) ;
#730 = CARTESIAN_POINT ( 'NONE',  ( 2.000000000000000000, 1.773042676681340968, -1.951563910473907981E-15 ) ) ;
#731 = DIRECTION ( 'NONE',  ( 0.000000000000000000, -1.000000000000000000, 0.000000000000000000 ) ) ;
#732 =( BOUNDED_CURVE ( )  B_SPLINE_CURVE ( 2, ( #402, #3161, #7865, #3114, #1829, #4510, #7198, #528, #4072 ),
 .UNSPECIFIED., .F., .T. ) 
 B_SPLINE_CURVE_WITH_KNOTS ( ( 3, 2, 2, 2, 3 ),
 ( 0.1428571428571428215, 0.1607142857142856984, 0.1785714285714285476, 0.1964285714285714246, 0.2142857142857142738 ),
 .UNSPECIFIED. ) 
 CURVE ( )  GEOMETRIC_REPRESENTATION_ITEM ( )  RATIONAL_B_SPLINE_CURVE ( ( 1.000000000000000222, 0.9238795325112866275, 1.000000000000000000, 0.9238795325112867385, 1.000000000000000000, 0.9238795325112867385, 1.000000000000000000, 0.9238795325112867385, 1.000000000000000000 ) ) 
 REPRESENTATION_ITEM ( '' )  );
#733 = ORIENTED_EDGE ( 'NONE', *, *, #8138, .T. ) ;
#734 = CARTESIAN_POINT ( 'NONE',  ( -37.96330746473829976, -50.84999999999999432, -4.057507815433013754 ) ) ;
#735 = EDGE_CURVE ( 'NONE', #1784, #5916, #4447, .T. ) ;
#736 = CARTESIAN_POINT ( 'NONE',  ( -39.86591130483550671, -38.54999999999999716, 1.562606840307984468 ) ) ;
#737 = AXIS2_PLACEMENT_3D ( 'NONE', #1807, #7132, #4488 ) ;
#738 = ORIENTED_EDGE ( 'NONE', *, *, #5306, .T. ) ;
#739 = DIRECTION ( 'NONE',  ( 0.000000000000000000, 0.000000000000000000, 1.000000000000000000 ) ) ;
#740 = CARTESIAN_POINT ( 'NONE',  ( -4.566987299999998307, -44.99999999999997158, -97.84999999890752065 ) ) ;
#741 = CARTESIAN_POINT ( 'NONE',  ( 3.535533905932737309, -48.53553390593270933, -99.50000000000000000 ) ) ;
#742 = CARTESIAN_POINT ( 'NONE',  ( -28.51387258211773812, -43.80000000000000426, 9.383039235653802379 ) ) ;
#743 = CARTESIAN_POINT ( 'NONE',  ( 3.229347689422841228, -48.22934768942280925, -97.34999999890753486 ) ) ;
#744 = SURFACE_SIDE_STYLE ('',( #4672 ) ) ;
#745 = CARTESIAN_POINT ( 'NONE',  ( -22.06198138166579170, -42.35140427513057659, 4.107139971057695682 ) ) ;
#746 = EDGE_CURVE ( 'NONE', #2486, #6385, #6425, .T. ) ;
#747 = CARTESIAN_POINT ( 'NONE',  ( -4.999999999999998224, -42.92893218813448897, -95.04300000002184845 ) ) ;
#748 = CARTESIAN_POINT ( 'NONE',  ( -22.42644454439892598, -45.90000000000001279, -3.858919247786222861 ) ) ;
#749 = CARTESIAN_POINT ( 'NONE',  ( 25.32221232802729460, -46.77334385938312522, 11.59192968702632065 ) ) ;
#750 = CARTESIAN_POINT ( 'NONE',  ( 2.000000000000000000, -1.314525273895014276E-15, -1.535500000000000087 ) ) ;
#751 = AXIS2_PLACEMENT_3D ( 'NONE', #3944, #577, #5339 ) ;
#752 = APPLICATION_PROTOCOL_DEFINITION ( 'draft international standard', 'automotive_design', 1998, #5770 ) ;
#753 = ORIENTED_EDGE ( 'NONE', *, *, #7226, .F. ) ;
#754 = DIRECTION ( 'NONE',  ( -0.000000000000000000, -0.000000000000000000, 1.000000000000000000 ) ) ;
#755 =( REPRESENTATION_RELATIONSHIP ('NONE','NONE', #2265, #7373 ) REPRESENTATION_RELATIONSHIP_WITH_TRANSFORMATION ( #840 )SHAPE_REPRESENTATION_RELATIONSHIP( ) );
#756 = CARTESIAN_POINT ( 'NONE',  ( -31.56260684030781505, -49.95000000000000995, 9.865911304835510265 ) ) ;
#757 = CARTESIAN_POINT ( 'NONE',  ( -38.83610826798580717, -49.55140427513056522, 1.343104241417631073 ) ) ;
#758 = DIRECTION ( 'NONE',  ( 0.000000000000000000, 0.000000000000000000, 1.000000000000000000 ) ) ;
#759 = FACE_OUTER_BOUND ( 'NONE', #5969, .T. ) ;
#760 = CARTESIAN_POINT ( 'NONE',  ( -31.50758917197619979, -47.94859572486943478, 9.874625247442176956 ) ) ;
#761 = CARTESIAN_POINT ( 'NONE',  ( 34.00000000000000000, 0.000000000000000000, 0.000000000000000000 ) ) ;
#762 = CYLINDRICAL_SURFACE ( 'NONE', #8087, 1.649999999999998579 ) ;
#763 =( NAMED_UNIT ( * ) PLANE_ANGLE_UNIT ( ) SI_UNIT ( $, .RADIAN. ) );
#764 = VERTEX_POINT ( 'NONE', #5766 ) ;
#765 = CARTESIAN_POINT ( 'NONE',  ( 4.999999999999998224, -44.99999999999997158, -98.60000000000000853 ) ) ;
#766 = EDGE_LOOP ( 'NONE', ( #3607, #2663 ) ) ;
#767 = CARTESIAN_POINT ( 'NONE',  ( -34.10713997105786888, -34.14859572486943051, -7.938018618334151455 ) ) ;
#768 = CARTESIAN_POINT ( 'NONE',  ( -39.85719736222883824, -42.54859572486944330, 1.617624508639602388 ) ) ;
#769 = CARTESIAN_POINT ( 'NONE',  ( -21.51138689804841420, -38.90140427513058086, -4.265706762501151772 ) ) ;
#770 = ORIENTED_EDGE ( 'NONE', *, *, #6382, .T. ) ;
#771 = EDGE_CURVE ( 'NONE', #772, #7794, #6358, .T. ) ;
#772 = VERTEX_POINT ( 'NONE', #3873 ) ;
#773 = CARTESIAN_POINT ( 'NONE',  ( -4.566987299999998307, -44.99999999999997158, -100.0499999989075235 ) ) ;
#774 = CARTESIAN_POINT ( 'NONE',  ( -26.64110105645932336, -9.999999999999998224, -24.00000000000000000 ) ) ;
#775 = CARTESIAN_POINT ( 'NONE',  ( -2.071067811865475505, -49.99999999999996447, -98.74999999781503845 ) ) ;
#776 = DIRECTION ( 'NONE',  ( -1.000000000000000000, 0.000000000000000000, 0.000000000000000000 ) ) ;
#777 = CARTESIAN_POINT ( 'NONE',  ( 0.1999999999999987899, 0.000000000000000000, 0.000000000000000000 ) ) ;
#778 = EDGE_CURVE ( 'NONE', #6845, #1128, #7172, .T. ) ;
#779 = EDGE_LOOP ( 'NONE', ( #8638, #5179, #3636, #2635 ) ) ;
#780 = CARTESIAN_POINT ( 'NONE',  ( -22.01140368885771892, -32.34859572486942625, 4.007875659808335378 ) ) ;
#781 = CARTESIAN_POINT ( 'NONE',  ( -21.53543802021056663, -33.90000000000000568, -4.312909747525783821 ) ) ;
#782 = AXIS2_PLACEMENT_3D ( 'NONE', #1939, #5036, #8351 ) ;
#783 = ORIENTED_EDGE ( 'NONE', *, *, #3043, .F. ) ;
#784 = DIRECTION ( 'NONE',  ( 0.000000000000000000, 0.000000000000000000, 1.000000000000000000 ) ) ;
#785 = CARTESIAN_POINT ( 'NONE',  ( -1.891708078845683705, -49.56698729999997255, -98.49999999890752633 ) ) ;
#786 = EDGE_CURVE ( 'NONE', #5319, #2418, #5107, .T. ) ;
#787 = CARTESIAN_POINT ( 'NONE',  ( 4.999999999999998224, -42.92893218813448897, -100.0499999978150356 ) ) ;
#788 = CARTESIAN_POINT ( 'NONE',  ( -20.13408869516453947, -49.04999999999999716, -1.562606840307983136 ) ) ;
#789 = CARTESIAN_POINT ( 'NONE',  ( 3.229347689422841228, -48.22934768942280925, -98.14999999890753202 ) ) ;
#790 = PLANE ( 'NONE',  #5639 ) ;
#791 = CARTESIAN_POINT ( 'NONE',  ( -38.38706344316003793, -40.70140427513058512, -1.382017864820032083 ) ) ;
#792 = TOROIDAL_SURFACE ( 'NONE', #4457, 3.299999999999999822, 0.2000000000000000111 ) ;
#793 = EDGE_CURVE ( 'NONE', #5525, #6251, #3781, .T. ) ;
#794 = CARTESIAN_POINT ( 'NONE',  ( 3.535533905932736420, -41.46446609406723383, -99.29300000002184845 ) ) ;
#795 = CARTESIAN_POINT ( 'NONE',  ( -37.57355545560112375, -47.40000000000001279, 3.858919247786223305 ) ) ;
#796 = ADVANCED_FACE ( 'NONE', ( #3827 ), #6507, .T. ) ;
#797 = FACE_OUTER_BOUND ( 'NONE', #8191, .T. ) ;
#798 = APPLICATION_PROTOCOL_DEFINITION ( 'draft international standard', 'automotive_design', 1998, #6216 ) ;
#799 = VERTEX_POINT ( 'NONE', #8543 ) ;
#800 = CARTESIAN_POINT ( 'NONE',  ( 4.999999999999998224, -44.99999999999997158, -100.0999999978150470 ) ) ;
#801 = VECTOR ( 'NONE', #7421, 1000.000000000000000 ) ;
#802 = CARTESIAN_POINT ( 'NONE',  ( -31.56260684030781505, -43.95000000000000284, 9.865911304835510265 ) ) ;
#803 = EDGE_CURVE ( 'NONE', #4035, #3309, #1727, .T. ) ;
#804 = CARTESIAN_POINT ( 'NONE',  ( -23.64089511245930098, -44.75140427513058228, -6.280328284105564762 ) ) ;
#805 = CARTESIAN_POINT ( 'NONE',  ( 29.67102067851989844, -40.00000000000000000, 12.49999999999996980 ) ) ;
#806 = DIRECTION ( 'NONE',  ( 1.000000000000000000, 0.000000000000000000, -0.000000000000000000 ) ) ;
#807 = CARTESIAN_POINT ( 'NONE',  ( -23.24502507771338600, -50.49859572486944614, 6.680053920257780220 ) ) ;
#808 = CARTESIAN_POINT ( 'NONE',  ( 3.535533969928884801, -41.46446615806338087, -100.0000000000000142 ) ) ;
#809 = CARTESIAN_POINT ( 'NONE',  ( -28.51387258211773812, -31.80000000000000782, 9.383039235653802379 ) ) ;
#810 = ORIENTED_EDGE ( 'NONE', *, *, #4569, .F. ) ;
#811 = CARTESIAN_POINT ( 'NONE',  ( 2.071067811865477282, -49.99999999999997158, -98.75000000000001421 ) ) ;
#812 = ORIENTED_EDGE ( 'NONE', *, *, #2573, .F. ) ;
#813 = CARTESIAN_POINT ( 'NONE',  ( -22.01140368885771892, -41.34859572486944757, 4.007875659808335378 ) ) ;
#814 = CARTESIAN_POINT ( 'NONE',  ( -20.60867331244750034, -38.19859572486942767, 1.433802505903951419 ) ) ;
#815 = CARTESIAN_POINT ( 'NONE',  ( -39.37475178375516549, -40.70140427513058512, -1.538452329860249712 ) ) ;
#816 = ORIENTED_EDGE ( 'NONE', *, *, #1726, .T. ) ;
#817 = CARTESIAN_POINT ( 'NONE',  ( 4.566987299999998307, -43.10829192115428299, -97.19999999890751496 ) ) ;
#818 = EDGE_CURVE ( 'NONE', #7794, #1195, #3435, .T. ) ;
#819 = DIRECTION ( 'NONE',  ( -1.224646799147353207E-16, 1.000000000000000000, 0.000000000000000000 ) ) ;
#820 = LINE ( 'NONE', #2774, #3625 ) ;
#821 = CARTESIAN_POINT ( 'NONE',  ( 3.229347689422839895, -41.77065231057713390, -97.34999999890752065 ) ) ;
#822 = CARTESIAN_POINT ( 'NONE',  ( -30.00000000000002842, 0.000000000000000000, -40.35000000000000142 ) ) ;
#823 = FACE_BOUND ( 'NONE', #7168, .T. ) ;
#824 = ORIENTED_EDGE ( 'NONE', *, *, #8649, .T. ) ;
#825 = CARTESIAN_POINT ( 'NONE',  ( -37.98859631114233792, -33.84859572486942625, -4.007875659808334490 ) ) ;
#826 = CARTESIAN_POINT ( 'NONE',  ( -28.43739315969223824, -36.45000000000000284, -9.865911304835512041 ) ) ;
#827 = ORIENTED_EDGE ( 'NONE', *, *, #612, .F. ) ;
#828 = CARTESIAN_POINT ( 'NONE',  ( -31.48612741788231517, -48.30000000000001137, -9.383039235653804155 ) ) ;
#829 = DIRECTION ( 'NONE',  ( 0.000000000000000000, 0.000000000000000000, 1.000000000000000000 ) ) ;
#830 = CARTESIAN_POINT ( 'NONE',  ( -33.35889894354067309, -7.999999999999996447, -23.99999999999999289 ) ) ;
#831 = DIRECTION ( 'NONE',  ( -0.000000000000000000, 0.000000000000000000, 1.000000000000000000 ) ) ;
#832 = CARTESIAN_POINT ( 'NONE',  ( 3.229347689422841228, -48.22934768942280925, -98.94999999890752918 ) ) ;
#833 = CARTESIAN_POINT ( 'NONE',  ( -33.90612223281073057, -43.10140427513058370, 7.549504333439023718 ) ) ;
#834 = EDGE_CURVE ( 'NONE', #4208, #4354, #6639, .T. ) ;
#835 = CARTESIAN_POINT ( 'NONE',  ( -2.071067811865475061, -39.99999999999997158, -95.15000000000000568 ) ) ;
#836 = CARTESIAN_POINT ( 'NONE',  ( 4.566987299999998307, -44.99999999999997158, -96.44999999890752918 ) ) ;
#837 = CARTESIAN_POINT ( 'NONE',  ( -34.05750781543319050, -48.15000000000001279, -7.963307464738194952 ) ) ;
#838 = AXIS2_PLACEMENT_3D ( 'NONE', #8397, #5741, #2402 ) ;
#839 = DIRECTION ( 'NONE',  ( 0.000000000000000000, -1.000000000000000000, 8.560894001270036306E-16 ) ) ;
#840 = ITEM_DEFINED_TRANSFORMATION ( 'NONE', 'NONE', #571,  #2554 ) ;
#841 =( NAMED_UNIT ( * ) PLANE_ANGLE_UNIT ( ) SI_UNIT ( $, .RADIAN. ) );
#842 = DIRECTION ( 'NONE',  ( 0.000000000000000000, 0.000000000000000000, 1.000000000000000000 ) ) ;
#843 = CARTESIAN_POINT ( 'NONE',  ( -36.31971658582311591, -41.25000000000000711, 6.319716585823199395 ) ) ;
#844 = AXIS2_PLACEMENT_3D ( 'NONE', #761, #1599, #2184 ) ;
#845 = CARTESIAN_POINT ( 'NONE',  ( 25.16326641152763344, -43.69081521296084958, 11.52653374317613455 ) ) ;
#846 = DIRECTION ( 'NONE',  ( -0.000000000000000000, 1.000000000000000000, -0.000000000000000000 ) ) ;
#847 = CARTESIAN_POINT ( 'NONE',  ( -38.44051085762733777, -42.39859572486944472, 4.360112732550414982 ) ) ;
#848 = CARTESIAN_POINT ( 'NONE',  ( 2.000000000000000000, -1.329782007511005837, 0.7677500000000023750 ) ) ;
#849 = CIRCLE ( 'NONE', #6478, 10.00000000000000178 ) ;
#850 = CARTESIAN_POINT ( 'NONE',  ( -31.56260684030781505, -34.95000000000000995, 9.865911304835508489 ) ) ;
#851 = ORIENTED_EDGE ( 'NONE', *, *, #4407, .F. ) ;
#852 = PLANE ( 'NONE',  #1788 ) ;
#853 = ORIENTED_EDGE ( 'NONE', *, *, #886, .F. ) ;
#854 = CARTESIAN_POINT ( 'NONE',  ( -37.98859631114233792, -39.84859572486944046, -4.007875659808334490 ) ) ;
#855 = CARTESIAN_POINT ( 'NONE',  ( -37.02382435302582309, -51.24859572486943193, 7.102600956461226467 ) ) ;
#856 = CARTESIAN_POINT ( 'NONE',  ( -34.00787565980851213, -29.15140427513058441, -7.988596311142238449 ) ) ;
#857 = AXIS2_PLACEMENT_3D ( 'NONE', #3752, #2969, #5644 ) ;
#858 = VERTEX_POINT ( 'NONE', #591 ) ;
#859 = CARTESIAN_POINT ( 'NONE',  ( -20.00000000000002487, 0.000000000000000000, -41.34999999999999432 ) ) ;
#860 = DIRECTION ( 'NONE',  ( 0.000000000000000000, 0.000000000000000000, 1.000000000000000000 ) ) ;
#861 = CARTESIAN_POINT ( 'NONE',  ( -2.796473189345805913E-16, -40.43301269999997061, -98.04999999890752349 ) ) ;
#862 = CARTESIAN_POINT ( 'NONE',  ( -30.00000000000002487, 0.000000000000000000, -29.65000000000000213 ) ) ;
#863 = DIRECTION ( 'NONE',  ( 1.000000000000000000, 0.000000000000000000, 0.000000000000000000 ) ) ;
#864 = VERTEX_POINT ( 'NONE', #1218 ) ;
#865 =( GEOMETRIC_REPRESENTATION_CONTEXT ( 3 ) GLOBAL_UNCERTAINTY_ASSIGNED_CONTEXT ( ( #8028 ) ) GLOBAL_UNIT_ASSIGNED_CONTEXT ( ( #490, #6581, #1919 ) ) REPRESENTATION_CONTEXT ( 'NONE', 'WORKASPACE' ) );
#866 = CARTESIAN_POINT ( 'NONE',  ( -36.01040764008574513, -51.00000000000000711, -6.010407640085605685 ) ) ;
#867 = CARTESIAN_POINT ( 'NONE',  ( -38.46456197978948666, -47.40000000000001279, 4.312909747525784709 ) ) ;
#868 = EDGE_LOOP ( 'NONE', ( #8063, #1620, #467 ) ) ;
#869 = CARTESIAN_POINT ( 'NONE',  ( -21.53543802021056663, -45.90000000000001279, -4.312909747525783821 ) ) ;
#870 = AXIS2_PLACEMENT_3D ( 'NONE', #8443, #981, #7818 ) ;
#871 = CARTESIAN_POINT ( 'NONE',  ( 50.00000000000002842, 30.00000000000000000, 80.00000000000002842 ) ) ;
#872 = CARTESIAN_POINT ( 'NONE',  ( -3.229347689422840784, -41.77065231057713390, -100.3499999989075206 ) ) ;
#873 = CARTESIAN_POINT ( 'NONE',  ( -4.999999999999998224, -42.92893218813448897, -98.94999999781504130 ) ) ;
#874 = CARTESIAN_POINT ( 'NONE',  ( -41.99999999999996447, 22.00000000000000000, 60.00000000000002842 ) ) ;
#875 = CARTESIAN_POINT ( 'NONE',  ( -1.891708078845683483, -49.56698729999997255, -97.49999999890754054 ) ) ;
#876 = VERTEX_POINT ( 'NONE', #8711 ) ;
#877 = CARTESIAN_POINT ( 'NONE',  ( -34.00787565980851213, -47.15140427513058086, -7.988596311142238449 ) ) ;
#878 = CIRCLE ( 'NONE', #6363, 2.149999999999985256 ) ;
#879 = CARTESIAN_POINT ( 'NONE',  ( -4.999999999999997335, -47.07106781186546129, -98.14300000002184277 ) ) ;
#880 = VECTOR ( 'NONE', #8032, 1000.000000000000000 ) ;
#881 = AXIS2_PLACEMENT_3D ( 'NONE', #1764, #2549, #8503 ) ;
#882 = CARTESIAN_POINT ( 'NONE',  ( -31.39812190974910422, -46.94999999999999574, 8.827394325379140483 ) ) ;
#883 = CARTESIAN_POINT ( 'NONE',  ( -30.00000000000000000, 60.00000000000002842, 12.49999999999998757 ) ) ;
#884 = PRODUCT_CONTEXT ( 'NONE', #2293, 'mechanical' ) ;
#885 = CARTESIAN_POINT ( 'NONE',  ( -41.99999999999996447, 48.00000000000002842, -23.64999999999999858 ) ) ;
#886 = EDGE_CURVE ( 'NONE', #2202, #3619, #5942, .T. ) ;
#887 = CARTESIAN_POINT ( 'NONE',  ( -22.42644454439892598, -33.90000000000000568, -3.858919247786222861 ) ) ;
#888 = AXIS2_PLACEMENT_3D ( 'NONE', #1840, #2501, #538 ) ;
#889 = PRODUCT_DEFINITION_SHAPE ( 'NONE', 'NONE',  #8725 ) ;
#890 = LINE ( 'NONE', #8264, #2347 ) ;
#891 = CARTESIAN_POINT ( 'NONE',  ( 0.000000000000000000, -44.99999999999997158, -95.00000000000000000 ) ) ;
#892 = CARTESIAN_POINT ( 'NONE',  ( -25.46513832392765408, -31.65000000000000568, 8.900167166472096270 ) ) ;
#893 = EDGE_CURVE ( 'NONE', #4571, #5715, #1301, .T. ) ;
#894 = CARTESIAN_POINT ( 'NONE',  ( 19.99999999999997513, 1.224646799147352901E-14, 60.00000000000002842 ) ) ;
#895 = CARTESIAN_POINT ( 'NONE',  ( -21.53543802021056663, -30.90000000000000924, -4.312909747525783821 ) ) ;
#896 =( LENGTH_UNIT ( ) NAMED_UNIT ( * ) SI_UNIT ( .MILLI., .METRE. ) );
#897 = EDGE_LOOP ( 'NONE', ( #6623, #5315 ) ) ;
#898 = DIRECTION ( 'NONE',  ( 0.000000000000000000, 0.8660254037844380415, -0.5000000000000012212 ) ) ;
#899 = VERTEX_POINT ( 'NONE', #5351 ) ;
#900 = CARTESIAN_POINT ( 'NONE',  ( -38.40363834695740053, -36.69859572486944188, -1.277368040863739118 ) ) ;
#901 = CARTESIAN_POINT ( 'NONE',  ( -25.41550616830297571, -44.64859572486944472, 8.874878320068054549 ) ) ;
#902 = CARTESIAN_POINT ( 'NONE',  ( -22.06198138166579170, -33.35140427513057659, 4.107139971057695682 ) ) ;
#903 = VECTOR ( 'NONE', #7606, 1000.000000000000000 ) ;
#904 = ADVANCED_FACE ( 'NONE', ( #6066 ), #8012, .F. ) ;
#905 = CARTESIAN_POINT ( 'NONE',  ( -1.891708078845683039, -40.43301269999998482, -100.1999999989075150 ) ) ;
#906 = DIRECTION ( 'NONE',  ( -1.000000000000000000, -0.000000000000000000, -0.000000000000000000 ) ) ;
#907 = CARTESIAN_POINT ( 'NONE',  ( -34.33209868862994796, -42.48249851487850748, 11.72687238757476003 ) ) ;
#908 = CARTESIAN_POINT ( 'NONE',  ( -3.229347689422840784, -41.77065231057713390, -97.14999999890753202 ) ) ;
#909 = LINE ( 'NONE', #6766, #903 ) ;
#910 = CARTESIAN_POINT ( 'NONE',  ( 4.999999999999998224, -44.99999999999997158, -96.09999999781504698 ) ) ;
#911 = EDGE_CURVE ( 'NONE', #6845, #2769, #1890, .T. ) ;
#912 = VERTEX_POINT ( 'NONE', #6680 ) ;
#913 = CARTESIAN_POINT ( 'NONE',  ( -21.59636165304264921, -38.19859572486942767, 1.277368040863740228 ) ) ;
#914 = CARTESIAN_POINT ( 'NONE',  ( -39.38303923565386100, -41.70000000000000995, -1.486127417882099788 ) ) ;
#915 = ORIENTED_EDGE ( 'NONE', *, *, #5570, .F. ) ;
#916 = EDGE_CURVE ( 'NONE', #5583, #5143, #1973, .T. ) ;
#917 = CARTESIAN_POINT ( 'NONE',  ( -39.86591130483550671, -44.55000000000001137, 1.562606840307984468 ) ) ;
#918 = CARTESIAN_POINT ( 'NONE',  ( -3.535533905932735532, -48.53553390593270933, -98.79999999781504982 ) ) ;
#919 = LINE ( 'NONE', #1532, #6968 ) ;
#920 = CARTESIAN_POINT ( 'NONE',  ( -4.999999999999998224, -44.99999999999997158, -98.09999999781504698 ) ) ;
#921 = CARTESIAN_POINT ( 'NONE',  ( 9.184850993605145972E-16, -49.99999999999997158, -97.89999999781504414 ) ) ;
#922 = CARTESIAN_POINT ( 'NONE',  ( -1.891708078845683483, -49.56698729999997255, -99.89999999890753202 ) ) ;
#923 = VERTEX_POINT ( 'NONE', #545 ) ;
#924 = CARTESIAN_POINT ( 'NONE',  ( -25.94249218456686279, -31.65000000000000568, 7.963307464738195840 ) ) ;
#925 = CIRCLE ( 'NONE', #7677, 1.649999999999998579 ) ;
#926 = EDGE_CURVE ( 'NONE', #4270, #282, #310, .T. ) ;
#927 = CARTESIAN_POINT ( 'NONE',  ( -3.535533905932736864, -41.46446609406723383, -99.89300000002185698 ) ) ;
#928 = CARTESIAN_POINT ( 'NONE',  ( 4.566987299999998307, -43.10829192115428299, -95.59999999890754907 ) ) ;
#929 = ADVANCED_FACE ( 'NONE', ( #6725 ), #3255, .F. ) ;
#930 = CARTESIAN_POINT ( 'NONE',  ( 5.000000000000000000, -47.07106781186545419, -96.94999999781504130 ) ) ;
#931 = CARTESIAN_POINT ( 'NONE',  ( -40.00000000000002842, 1.224646799147353059E-15, -26.00000000000000355 ) ) ;
#932 = TOROIDAL_SURFACE ( 'NONE', #1494, 2.000000000000000000, 1.000000000000000000 ) ;
#933 = DIRECTION ( 'NONE',  ( -0.000000000000000000, 1.000000000000000000, 1.224646799147353207E-16 ) ) ;
#934 = CARTESIAN_POINT ( 'NONE',  ( -37.96330746473829976, -35.84999999999998721, -4.057507815433013754 ) ) ;
#935 = CARTESIAN_POINT ( 'NONE',  ( -26.02663761693602495, -41.94765302695305564, 11.85321826485150432 ) ) ;
#936 = FACE_OUTER_BOUND ( 'NONE', #5015, .T. ) ;
#937 = CARTESIAN_POINT ( 'NONE',  ( -36.71751442127229836, -36.00000000000000711, -6.717514421272142044 ) ) ;
#938 = DIRECTION ( 'NONE',  ( -0.000000000000000000, -0.000000000000000000, -1.000000000000000000 ) ) ;
#939 = CARTESIAN_POINT ( 'NONE',  ( -34.31290974752564438, -41.10000000000000142, 8.464561979789547053 ) ) ;
#940 = ORIENTED_EDGE ( 'NONE', *, *, #4323, .F. ) ;
#941 = CARTESIAN_POINT ( 'NONE',  ( 2.000000000000000000, 1.773042676681340968, -1.951563910473907981E-15 ) ) ;
#942 = ORIENTED_EDGE ( 'NONE', *, *, #4836, .T. ) ;
#943 = CARTESIAN_POINT ( 'NONE',  ( -31.38201786482021305, -37.29859572486943620, -8.387063443159975762 ) ) ;
#944 = CARTESIAN_POINT ( 'NONE',  ( -22.97617564697422665, -46.74859572486943904, -7.102600956461224690 ) ) ;
#945 = CARTESIAN_POINT ( 'NONE',  ( -28.54686042191934092, -29.45140427513057801, -8.818680382772479120 ) ) ;
#946 = AXIS2_PLACEMENT_3D ( 'NONE', #774, #5439, #860 ) ;
#947 = CIRCLE ( 'NONE', #3762, 1.649999999999998579 ) ;
#948 = CARTESIAN_POINT ( 'NONE',  ( -2.796473189345805913E-16, -40.43301269999997061, -97.84999999890753486 ) ) ;
#949 = DIRECTION ( 'NONE',  ( -0.000000000000000000, -0.000000000000000000, 1.000000000000000000 ) ) ;
#950 = CARTESIAN_POINT ( 'NONE',  ( -26.64110105645932336, -8.999999999999998224, -24.00000000000000000 ) ) ;
#951 = CARTESIAN_POINT ( 'NONE',  ( -3.229347689422839451, -48.22934768942280925, -97.74999999890751212 ) ) ;
#952 = DIRECTION ( 'NONE',  ( 0.000000000000000000, 0.000000000000000000, 1.000000000000000000 ) ) ;
#953 = CARTESIAN_POINT ( 'NONE',  ( 4.566987299999998307, -43.10829192115428299, -96.59999999890753486 ) ) ;
#954 = LINE ( 'NONE', #2655, #1137 ) ;
#955 = ORIENTED_EDGE ( 'NONE', *, *, #6438, .T. ) ;
#956 = CARTESIAN_POINT ( 'NONE',  ( -28.65689575858256077, -40.44859572486944188, -8.836108267985801845 ) ) ;
#957 = CARTESIAN_POINT ( 'NONE',  ( -25.46513832392765408, -46.65000000000001279, 8.900167166472096270 ) ) ;
#958 = CIRCLE ( 'NONE', #517, 2.149999999999985256 ) ;
#959 = EDGE_LOOP ( 'NONE', ( #4655, #2762 ) ) ;
#960 = CARTESIAN_POINT ( 'NONE',  ( -20.12537475255788522, -30.05140427513057944, -1.507589171976365439 ) ) ;
#961 = LINE ( 'NONE', #3740, #2648 ) ;
#962 = DIRECTION ( 'NONE',  ( -1.000000000000000000, -0.000000000000000000, -0.000000000000000000 ) ) ;
#963 = CARTESIAN_POINT ( 'NONE',  ( -4.999999999999998224, -44.99999999999997158, -99.69999999781505551 ) ) ;
#964 = CARTESIAN_POINT ( 'NONE',  ( -34.35889894354067309, -8.999999999999998224, -24.00000000000000000 ) ) ;
#965 = CARTESIAN_POINT ( 'NONE',  ( 4.566987299999998307, -44.99999999999997158, -98.84999999890753486 ) ) ;
#966 = ADVANCED_FACE ( 'NONE', ( #7257 ), #6764, .T. ) ;
#967 = ORIENTED_EDGE ( 'NONE', *, *, #158, .F. ) ;
#968 = CARTESIAN_POINT ( 'NONE',  ( -31.45313957808072303, -48.95140427513057091, 8.818680382772479120 ) ) ;
#969 = PRODUCT_DEFINITION_SHAPE ( 'NONE', 'NONE',  #8723 ) ;
#970 = CARTESIAN_POINT ( 'NONE',  ( -3.535533905932736864, -41.46446609406723383, -98.29300000002184845 ) ) ;
#971 = CARTESIAN_POINT ( 'NONE',  ( -41.99999999999996447, 60.00000000000002842, 20.35000000000000142 ) ) ;
#972 = CARTESIAN_POINT ( 'NONE',  ( 4.999999999999998224, -44.99999999999997158, -97.69999999781505551 ) ) ;
#973 = DIRECTION ( 'NONE',  ( 0.000000000000000000, 0.000000000000000000, 1.000000000000000000 ) ) ;
#974 =( LENGTH_UNIT ( ) NAMED_UNIT ( * ) SI_UNIT ( .MILLI., .METRE. ) );
#975 = CARTESIAN_POINT ( 'NONE',  ( -37.96330746473829976, -38.85000000000001563, -4.057507815433013754 ) ) ;
#976 = LINE ( 'NONE', #7930, #6829 ) ;
#977 = CARTESIAN_POINT ( 'NONE',  ( -36.01040764008574513, -30.00000000000000711, -6.010407640085605685 ) ) ;
#978 = CARTESIAN_POINT ( 'NONE',  ( -28.43739315969223824, -30.44999999999999574, -9.865911304835512041 ) ) ;
#979 = DIRECTION ( 'NONE',  ( 0.000000000000000000, 1.000000000000000000, -1.467581828789149335E-15 ) ) ;
#980 = CARTESIAN_POINT ( 'NONE',  ( -28.43739315969223824, -45.45000000000000284, -9.865911304835512041 ) ) ;
#981 = DIRECTION ( 'NONE',  ( 0.000000000000000000, 0.000000000000000000, 1.000000000000000000 ) ) ;
#982 = ORIENTED_EDGE ( 'NONE', *, *, #7961, .F. ) ;
#983 = ORIENTED_EDGE ( 'NONE', *, *, #2920, .F. ) ;
#984 = CARTESIAN_POINT ( 'NONE',  ( -31.34310424141748896, -35.94859572486944188, 8.836108267985801845 ) ) ;
#985 = CARTESIAN_POINT ( 'NONE',  ( -39.85719736222883824, -45.54859572486944330, 1.617624508639602388 ) ) ;
#986 = CARTESIAN_POINT ( 'NONE',  ( -25.63988726744978663, -47.60140427513058370, -8.440510857627391061 ) ) ;
#987 = CARTESIAN_POINT ( 'NONE',  ( -1.891708078845683705, -49.56698729999997255, -99.09999999890753486 ) ) ;
#988 = B_SPLINE_CURVE_WITH_KNOTS ( 'NONE', 3,
 ( #3772, #7077, #5751, #3162, #1036, #2329, #5007, #7696, #3075, #403, #8450, #443, #5836, #2492, #5173, #4512, #8089, #7329, #1955, #5292, #8613, #1873 ),
 .UNSPECIFIED., .F., .F.,
 ( 4, 2, 2, 2, 2, 2, 2, 2, 2, 2, 4 ),
 ( 0.01579945264986103853, 0.01629290087626464323, 0.01678634910266824792, 0.01777324555547545731, 0.01876014200828266323, 0.01974703846108986915, 0.02073393491389707508, 0.02122738314030068324, 0.02172083136670428793, 0.02270772781951150079, 0.02369462427231871365 ),
 .UNSPECIFIED. ) ;
#989 = CARTESIAN_POINT ( 'NONE',  ( -26.64110105645932336, 9.000000000000001776, -24.00000000000000000 ) ) ;
#990 = PRODUCT_DEFINITION_SHAPE ( 'NONE', 'NONE',  #1843 ) ;
#991 = DIRECTION ( 'NONE',  ( -0.000000000000000000, 1.000000000000000000, -0.000000000000000000 ) ) ;
#992 = CARTESIAN_POINT ( 'NONE',  ( -26.23382588360912848, -48.30471456237976469, 11.92153802757356118 ) ) ;
#993 = CARTESIAN_POINT ( 'NONE',  ( -4.566987299999998307, -43.10829192115428299, -97.89999999890751781 ) ) ;
#994 = ORIENTED_EDGE ( 'NONE', *, *, #4575, .T. ) ;
#995 = EDGE_CURVE ( 'NONE', #5982, #8204, #1392, .T. ) ;
#996 = CARTESIAN_POINT ( 'NONE',  ( -38.40363834695740053, -42.69859572486944188, -1.277368040863739118 ) ) ;
#997 = CARTESIAN_POINT ( 'NONE',  ( -20.61696076434619584, -43.20000000000000995, 1.486127417882100676 ) ) ;
#998 = CIRCLE ( 'NONE', #4381, 1.000000000000000888 ) ;
#999 = VERTEX_POINT ( 'NONE', #7967 ) ;
#1000 = CARTESIAN_POINT ( 'NONE',  ( -36.68005392025794009, -38.00140427513057517, -6.754974922286504757 ) ) ;
#1001 = DIRECTION ( 'NONE',  ( 1.000000000000000000, 0.000000000000000000, 0.000000000000000000 ) ) ;
#1002 = LINE ( 'NONE', #8423, #4723 ) ;
#1003 = DIRECTION ( 'NONE',  ( -1.000000000000000000, -6.123233995736960786E-17, 0.000000000000000000 ) ) ;
#1004 =( GEOMETRIC_REPRESENTATION_CONTEXT ( 3 ) GLOBAL_UNCERTAINTY_ASSIGNED_CONTEXT ( ( #3687 ) ) GLOBAL_UNIT_ASSIGNED_CONTEXT ( ( #7291, #1426, #2761 ) ) REPRESENTATION_CONTEXT ( 'NONE', 'WORKASPACE' ) );
#1005 = DIRECTION ( 'NONE',  ( -1.000000000000000000, 0.000000000000000000, 0.000000000000000000 ) ) ;
#1006 = CARTESIAN_POINT ( 'NONE',  ( 9.184850993605145972E-16, -49.99999999999997158, -95.60000000000000853 ) ) ;
#1007 = EDGE_CURVE ( 'NONE', #4525, #7472, #6705, .T. ) ;
#1008 = EDGE_CURVE ( 'NONE', #6235, #8538, #3206, .T. ) ;
#1009 = VERTEX_POINT ( 'NONE', #4000 ) ;
#1010 = CARTESIAN_POINT ( 'NONE',  ( -37.57355545560112375, -35.40000000000000568, 3.858919247786223305 ) ) ;
#1011 = CARTESIAN_POINT ( 'NONE',  ( 4.999999999999998224, -44.99999999999997158, -99.40000000000000568 ) ) ;
#1012 = ORIENTED_EDGE ( 'NONE', *, *, #6438, .F. ) ;
#1014 = CIRCLE ( 'NONE', #1437, 9.999999999999994671 ) ;
#1013 = CARTESIAN_POINT ( 'NONE',  ( 8.389419568037416259E-16, -49.56698729999997255, -95.84999999890753486 ) ) ;
#1015 = CARTESIAN_POINT ( 'NONE',  ( 3.535533905932736420, -41.46446609406723383, -97.59999999781504698 ) ) ;
#1016 = CIRCLE ( 'NONE', #1730, 12.49999999999998401 ) ;
#1017 = CARTESIAN_POINT ( 'NONE',  ( -11.32499999999999929, 0.000000000000000000, 0.000000000000000000 ) ) ;
#1018 = EDGE_CURVE ( 'NONE', #2059, #1305, #638, .T. ) ;
#1019 = DIRECTION ( 'NONE',  ( -0.000000000000000000, -0.000000000000000000, -1.000000000000000000 ) ) ;
#1020 = CARTESIAN_POINT ( 'NONE',  ( -25.94249218456686279, -43.64999999999999147, 7.963307464738195840 ) ) ;
#1021 = CIRCLE ( 'NONE', #5949, 1.000000000000000888 ) ;
#1022 = CYLINDRICAL_SURFACE ( 'NONE', #3219, 2.099999999999997868 ) ;
#1023 = CARTESIAN_POINT ( 'NONE',  ( 4.566987300000000083, -46.89170807884564596, -95.89999999890753202 ) ) ;
#1024 = DIRECTION ( 'NONE',  ( 0.000000000000000000, 0.000000000000000000, 1.000000000000000000 ) ) ;
#1025 = CARTESIAN_POINT ( 'NONE',  ( -31.56260684030781505, -37.94999999999998153, 9.865911304835510265 ) ) ;
#1026 = LINE ( 'NONE', #3103, #1095 ) ;
#1027 = CARTESIAN_POINT ( 'NONE',  ( -38.46456197978948666, -38.40000000000000568, 4.312909747525784709 ) ) ;
#1028 =( LENGTH_UNIT ( ) NAMED_UNIT ( * ) SI_UNIT ( .MILLI., .METRE. ) );
#1029 = ORIENTED_EDGE ( 'NONE', *, *, #2094, .F. ) ;
#1030 = AXIS2_PLACEMENT_3D ( 'NONE', #3905, #1084, #4520 ) ;
#1031 = EDGE_LOOP ( 'NONE', ( #6594, #5096, #4196, #1185 ) ) ;
#1032 = CARTESIAN_POINT ( 'NONE',  ( -21.59636165304264921, -50.19859572486944188, 1.277368040863740228 ) ) ;
#1033 = CARTESIAN_POINT ( 'NONE',  ( -23.24502507771338600, -47.49859572486944614, 6.680053920257780220 ) ) ;
#1034 = CARTESIAN_POINT ( 'NONE',  ( -33.90612223281073057, -31.10140427513058370, 7.549504333439023718 ) ) ;
#1035 = CARTESIAN_POINT ( 'NONE',  ( -4.999999999999998224, -44.99999999999997158, -95.00000000000000000 ) ) ;
#1036 = CARTESIAN_POINT ( 'NONE',  ( 30.82435085130693153, -40.06565635038678863, 12.47384660903967735 ) ) ;
#1037 = CARTESIAN_POINT ( 'NONE',  ( -38.90016716647221529, -38.85000000000001563, -4.534861676072185155 ) ) ;
#1038 = PLANE ( 'NONE',  #1408 ) ;
#1039 = CARTESIAN_POINT ( 'NONE',  ( -35.35889894354067309, 0.000000000000000000, -24.00000000000000000 ) ) ;
#1040 = CARTESIAN_POINT ( 'NONE',  ( 3.229347689422839895, -41.77065231057713390, -97.34999999890752065 ) ) ;
#1041 = FACE_BOUND ( 'NONE', #3210, .T. ) ;
#1042 = ORIENTED_EDGE ( 'NONE', *, *, #7811, .T. ) ;
#1043 = CARTESIAN_POINT ( 'NONE',  ( -34.10713997105786888, -37.14859572486943762, -7.938018618334151455 ) ) ;
#1044 = CIRCLE ( 'NONE', #6810, 10.00000000000000178 ) ;
#1045 = CARTESIAN_POINT ( 'NONE',  ( -28.51387258211773812, -43.80000000000000426, 9.383039235653802379 ) ) ;
#1046 = VERTEX_POINT ( 'NONE', #950 ) ;
#1047 = CARTESIAN_POINT ( 'NONE',  ( -36.68005392025794009, -35.00140427513057517, -6.754974922286504757 ) ) ;
#1048 = CARTESIAN_POINT ( 'NONE',  ( 0.000000000000000000, -44.99999999999997158, -95.00000000000000000 ) ) ;
#1049 = CYLINDRICAL_SURFACE ( 'NONE', #6547, 1.649999999999998579 ) ;
#1050 = CARTESIAN_POINT ( 'NONE',  ( -3.061616997868382155E-16, -39.99999999999997158, -97.49999999781503845 ) ) ;
#1051 = CARTESIAN_POINT ( 'NONE',  ( 50.00000000000002842, -59.99999999999997158, 30.00000000000000000 ) ) ;
#1052 = CARTESIAN_POINT ( 'NONE',  ( 2.071067811865474173, -39.99999999999997158, -96.04999999999999716 ) ) ;
#1053 = VERTEX_POINT ( 'NONE', #2859 ) ;
#1054 = CARTESIAN_POINT ( 'NONE',  ( -22.03669253526174998, -37.35000000000000853, 4.057507815433014642 ) ) ;
#1055 = EDGE_CURVE ( 'NONE', #6557, #4874, #820, .T. ) ;
#1056 = VERTEX_POINT ( 'NONE', #2815 ) ;
#1057 = CARTESIAN_POINT ( 'NONE',  ( 9.184850993605145972E-16, -49.99999999999997158, -98.79999999999999716 ) ) ;
#1058 = CARTESIAN_POINT ( 'NONE',  ( -3.535533905932735532, -48.53553390593270933, -97.99999999781503845 ) ) ;
#1059 = DIRECTION ( 'NONE',  ( 0.000000000000000000, 0.000000000000000000, -1.000000000000000000 ) ) ;
#1060 = VECTOR ( 'NONE', #1897, 1000.000000000000000 ) ;
#1061 = DIRECTION ( 'NONE',  ( 0.000000000000000000, 0.000000000000000000, 1.000000000000000000 ) ) ;
#1062 = PRODUCT ( 'Body', 'Body', '', ( #884 ) ) ;
#1063 = DIRECTION ( 'NONE',  ( -0.000000000000000000, 0.8660254037844392627, 0.4999999999999990008 ) ) ;
#1064 = EDGE_CURVE ( 'NONE', #7279, #8149, #6180, .T. ) ;
#1065 = CARTESIAN_POINT ( 'NONE',  ( -33.35889894354067309, 10.00000000000000178, -25.00000000000000000 ) ) ;
#1066 =( BOUNDED_SURFACE ( )  B_SPLINE_SURFACE ( 1, 2, ( 
 ( #1706, #4394, #3038, #1615, #4476, #332, #3648, #7162, #3816, #7083, #7743, #2333, #7120, #6326, #5841, #6455, #407, #4305, #2417, #5095, #1661, #2992, #5713, #953, #5137, #7700, #5669, #8371, #6371, #1755, #6497, #7829, #4352, #1082, #7786, #1122, #3079, #5013, #1040, #4437, #5798, #8531, #5053, #8414, #3120, #2378, #3776, #1794, #7032, #993, #3733, #8492, #2456, #449, #6414, #3691, #371, #4969, #5755, #6989, #3167, #7652, #291, #7955, #5927, #5888, #6052, #6621, #4606, #4563, #1333, #1918, #1247, #578, #8619, #3204, #7204, #4034, #8661, #624, #7913, #3945, #1959, #8574, #6712, #2587, #8700, #3903, #7871, #2538, #4646, #6010, #672, #7290, #2627, #8002, #1288, #5257, #5217, #3294, #2498 ),
 ( #5968, #5297, #1166, #3989, #7334, #3333, #6669, #4517, #1879, #3860, #2672, #5178, #5340, #7246, #8043, #2004, #488, #4696, #7381, #1207, #3378, #6580, #1835, #6539, #535, #3245, #2714, #2050, #4739, #5384, #8093, #14, #8681, #1358, #7359, #1313, #696, #6778, #2697, #6645, #6079, #602, #743, #5323, #3316, #5238, #4813, #7447, #4671, #7933, #5365, #4013, #1405, #3402, #8642, #4059, #3448, #4584, #8023, #8068, #1229, #6692, #2608, #5276, #2031, #1984, #37, #7980, #8596, #1942, #2740, #4719, #650, #3359, #8118, #4764, #7268, #5409, #557, #2561, #1900, #3268, #4627, #7311, #6737, #2076, #4101, #7403, #5948, #3926, #1268, #6601, #3968, #6034, #5990, #2654, #773, #8279, #7517, #905, #2241 ) ),
 .UNSPECIFIED., .F., .F., .T. ) 
 B_SPLINE_SURFACE_WITH_KNOTS ( ( 2, 2 ),
 ( 3, 2, 2, 2, 2, 2, 2, 2, 2, 2, 2, 2, 2, 2, 2, 2, 2, 2, 2, 2, 2, 2, 2, 2, 2, 2, 2, 2, 2, 2, 2, 2, 2, 2, 2, 2, 2, 2, 2, 2, 2, 2, 2, 2, 2, 2, 2, 2, 2, 2, 3 ),
 ( 0.000000000000000000, 1.000000000000000000 ),
 ( 0.000000000000000000, 0.01785714285714285615, 0.03571428571428571230, 0.05357142857142856845, 0.07142857142857142461, 0.08928571428571428770, 0.1071428571428571369, 0.1250000000000000000, 0.1428571428571428492, 0.1607142857142857262, 0.1785714285714285754, 0.1964285714285714246, 0.2142857142857142738, 0.2321428571428571508, 0.2500000000000000000, 0.2678571428571428492, 0.2857142857142856984, 0.3035714285714285476, 0.3214285714285714524, 0.3392857142857143016, 0.3571428571428571508, 0.3750000000000000000, 0.3928571428571428492, 0.4107142857142856984, 0.4285714285714285476, 0.4464285714285714524, 0.4642857142857143016, 0.4821428571428571508, 0.5000000000000000000, 0.5178571428571429047, 0.5357142857142856984, 0.5535714285714286031, 0.5714285714285713969, 0.5892857142857143016, 0.6071428571428570953, 0.6250000000000000000, 0.6428571428571429047, 0.6607142857142856984, 0.6785714285714286031, 0.6964285714285713969, 0.7142857142857143016, 0.7321428571428570953, 0.7500000000000000000, 0.7678571428571429047, 0.7857142857142856984, 0.8035714285714286031, 0.8214285714285713969, 0.8392857142857143016, 0.8571428571428570953, 0.8750000000000000000, 0.8928571428571429047 ),
 .UNSPECIFIED. ) 
 GEOMETRIC_REPRESENTATION_ITEM ( )  RATIONAL_B_SPLINE_SURFACE ( (
 ( 1.000000000000000000, 0.9238795325112867385, 1.000000000000000000, 0.9238795325112867385, 1.000000000000000000, 0.9238795325112867385, 1.000000000000000000, 0.9238795325112867385, 1.000000000000000000, 0.9238795325112867385, 1.000000000000000000, 0.9238795325112867385, 1.000000000000000000, 0.9238795325112867385, 1.000000000000000000, 0.9238795325112867385, 1.000000000000000000, 0.9238795325112867385, 1.000000000000000000, 0.9238795325112867385, 1.000000000000000000, 0.9238795325112867385, 1.000000000000000000, 0.9238795325112867385, 1.000000000000000000, 0.9238795325112867385, 1.000000000000000000, 0.9238795325112867385, 1.000000000000000000, 0.9238795325112867385, 1.000000000000000000, 0.9238795325112867385, 1.000000000000000000, 0.9238795325112867385, 1.000000000000000000, 0.9238795325112867385, 1.000000000000000000, 0.9238795325112867385, 1.000000000000000000, 0.9238795325112867385, 1.000000000000000000, 0.9238795325112867385, 1.000000000000000000, 0.9238795325112867385, 1.000000000000000000, 0.9238795325112867385, 1.000000000000000000, 0.9238795325112867385, 1.000000000000000000, 0.9238795325112867385, 1.000000000000000000, 0.9238795325112867385, 1.000000000000000000, 0.9238795325112867385, 1.000000000000000000, 0.9238795325112867385, 1.000000000000000000, 0.9238795325112867385, 1.000000000000000000, 0.9238795325112867385, 1.000000000000000000, 0.9238795325112867385, 1.000000000000000000, 0.9238795325112867385, 1.000000000000000000, 0.9238795325112867385, 1.000000000000000000, 0.9238795325112867385, 1.000000000000000000, 0.9238795325112867385, 1.000000000000000000, 0.9238795325112867385, 1.000000000000000000, 0.9238795325112867385, 1.000000000000000000, 0.9238795325112867385, 1.000000000000000000, 0.9238795325112867385, 1.000000000000000000, 0.9238795325112867385, 1.000000000000000000, 0.9238795325112867385, 1.000000000000000000, 0.9238795325112867385, 1.000000000000000000, 0.9238795325112867385, 1.000000000000000000, 0.9238795325112867385, 1.000000000000000000, 0.9238795325112867385, 1.000000000000000000, 0.9238795325112867385, 1.000000000000000000, 0.9238795325112867385, 1.000000000000000000, 0.9238795325112867385, 1.000000000000000000, 0.9238795325112867385, 1.000000000000000000, 0.9238795325112867385, 1.000000000000000000),
 ( 1.000000000000000000, 0.9238795325112867385, 1.000000000000000000, 0.9238795325112867385, 1.000000000000000000, 0.9238795325112867385, 1.000000000000000000, 0.9238795325112867385, 1.000000000000000000, 0.9238795325112867385, 1.000000000000000000, 0.9238795325112867385, 1.000000000000000000, 0.9238795325112867385, 1.000000000000000000, 0.9238795325112867385, 1.000000000000000000, 0.9238795325112867385, 1.000000000000000000, 0.9238795325112867385, 1.000000000000000000, 0.9238795325112867385, 1.000000000000000000, 0.9238795325112867385, 1.000000000000000000, 0.9238795325112867385, 1.000000000000000000, 0.9238795325112867385, 1.000000000000000000, 0.9238795325112867385, 1.000000000000000000, 0.9238795325112867385, 1.000000000000000000, 0.9238795325112867385, 1.000000000000000000, 0.9238795325112867385, 1.000000000000000000, 0.9238795325112867385, 1.000000000000000000, 0.9238795325112867385, 1.000000000000000000, 0.9238795325112867385, 1.000000000000000000, 0.9238795325112867385, 1.000000000000000000, 0.9238795325112867385, 1.000000000000000000, 0.9238795325112867385, 1.000000000000000000, 0.9238795325112867385, 1.000000000000000000, 0.9238795325112867385, 1.000000000000000000, 0.9238795325112867385, 1.000000000000000000, 0.9238795325112867385, 1.000000000000000000, 0.9238795325112867385, 1.000000000000000000, 0.9238795325112867385, 1.000000000000000000, 0.9238795325112867385, 1.000000000000000000, 0.9238795325112867385, 1.000000000000000000, 0.9238795325112867385, 1.000000000000000000, 0.9238795325112867385, 1.000000000000000000, 0.9238795325112867385, 1.000000000000000000, 0.9238795325112867385, 1.000000000000000000, 0.9238795325112867385, 1.000000000000000000, 0.9238795325112867385, 1.000000000000000000, 0.9238795325112867385, 1.000000000000000000, 0.9238795325112867385, 1.000000000000000000, 0.9238795325112867385, 1.000000000000000000, 0.9238795325112867385, 1.000000000000000000, 0.9238795325112867385, 1.000000000000000000, 0.9238795325112867385, 1.000000000000000000, 0.9238795325112867385, 1.000000000000000000, 0.9238795325112867385, 1.000000000000000000, 0.9238795325112867385, 1.000000000000000000, 0.9238795325112867385, 1.000000000000000000, 0.9238795325112867385, 1.000000000000000000, 0.9238795325112867385, 1.000000000000000000) ) ) 
 REPRESENTATION_ITEM ( '' )  SURFACE ( )  );
#1067 = CARTESIAN_POINT ( 'NONE',  ( 42.00000000000000711, 48.00000000000002842, 21.99999999999992184 ) ) ;
#1068 = CARTESIAN_POINT ( 'NONE',  ( -34.53486167607238144, -39.14999999999999147, -8.900167166472096270 ) ) ;
#1069 = DIRECTION ( 'NONE',  ( 0.000000000000000000, 0.000000000000000000, 1.000000000000000000 ) ) ;
#1070 = CARTESIAN_POINT ( 'NONE',  ( -39.38303923565386100, -38.70000000000000284, -1.486127417882099788 ) ) ;
#1071 = EDGE_CURVE ( 'NONE', #5205, #5875, #6198, .T. ) ;
#1072 = VERTEX_POINT ( 'NONE', #3758 ) ;
#1073 = CARTESIAN_POINT ( 'NONE',  ( -25.89286002894218086, -50.64859572486944472, 7.938018618334153231 ) ) ;
#1074 = CARTESIAN_POINT ( 'NONE',  ( -36.71751442127229836, -36.00000000000000711, -6.717514421272142044 ) ) ;
#1075 = CARTESIAN_POINT ( 'NONE',  ( -21.16389173201424612, -39.05140427513057944, -1.343104241417630185 ) ) ;
#1076 = VECTOR ( 'NONE', #3796, 1000.000000000000000 ) ;
#1077 = CARTESIAN_POINT ( 'NONE',  ( 8.389419568037416259E-16, -49.56698729999997255, -99.04999999890752349 ) ) ;
#1078 = DIRECTION ( 'NONE',  ( -1.000000000000000000, -1.224646799147352961E-16, 0.000000000000000000 ) ) ;
#1079 = CARTESIAN_POINT ( 'NONE',  ( -38.90016716647221529, -35.84999999999998721, -4.534861676072185155 ) ) ;
#1080 = CARTESIAN_POINT ( 'NONE',  ( 2.000000000000000000, 1.773042676681340968, -1.951563910473907981E-15 ) ) ;
#1081 = CARTESIAN_POINT ( 'NONE',  ( -49.99999999999997158, -59.99999999999997158, 30.00000000000000000 ) ) ;
#1082 = CARTESIAN_POINT ( 'NONE',  ( -4.566987299999998307, -43.10829192115428299, -97.09999999890752065 ) ) ;
#1083 = EDGE_LOOP ( 'NONE', ( #3654, #4068, #5069, #1575 ) ) ;
#1084 = DIRECTION ( 'NONE',  ( -0.000000000000000000, 0.000000000000000000, 1.000000000000000000 ) ) ;
#1085 = CARTESIAN_POINT ( 'NONE',  ( -36.28032828410546529, -45.24859572486943904, 6.359104887540839357 ) ) ;
#1086 = CARTESIAN_POINT ( 'NONE',  ( -39.86591130483550671, -50.55000000000001137, 1.562606840307984468 ) ) ;
#1087 = VECTOR ( 'NONE', #7029, 1000.000000000000000 ) ;
#1088 = ORIENTED_EDGE ( 'NONE', *, *, #6329, .T. ) ;
#1089 = VECTOR ( 'NONE', #1578, 1000.000000000000000 ) ;
#1090 = CARTESIAN_POINT ( 'NONE',  ( -25.63988726744978663, -35.60140427513057659, -8.440510857627391061 ) ) ;
#1091 = CARTESIAN_POINT ( 'NONE',  ( -30.00000000000000000, -49.99999999999997158, 12.49999999999997335 ) ) ;
#1092 = CARTESIAN_POINT ( 'NONE',  ( -25.64110105645932336, 8.000000000000000000, 125.0000000000000000 ) ) ;
#1093 = CARTESIAN_POINT ( 'NONE',  ( -4.999999999999998224, -44.99999999999997158, -95.79999999999999716 ) ) ;
#1094 = FACE_OUTER_BOUND ( 'NONE', #2864, .T. ) ;
#1095 = VECTOR ( 'NONE', #5784, 1000.000000000000000 ) ;
#1096 = CARTESIAN_POINT ( 'NONE',  ( 4.999999999999998224, -44.99999999999997158, -95.40000000000000568 ) ) ;
#1097 = ORIENTED_EDGE ( 'NONE', *, *, #3505, .F. ) ;
#1098 =( REPRESENTATION_RELATIONSHIP ('NONE','NONE', #2265, #4062 ) REPRESENTATION_RELATIONSHIP_WITH_TRANSFORMATION ( #2266 )SHAPE_REPRESENTATION_RELATIONSHIP( ) );
#1099 = CARTESIAN_POINT ( 'NONE',  ( -38.38706344316003793, -49.70140427513058512, -1.382017864820032083 ) ) ;
#1100 = VERTEX_POINT ( 'NONE', #4132 ) ;
#1101 = CARTESIAN_POINT ( 'NONE',  ( -3.535533905932736864, -41.46446609406723383, -99.10000000000000853 ) ) ;
#1102 = CARTESIAN_POINT ( 'NONE',  ( -38.82739432537914581, -50.55000000000001137, 1.398121909749243663 ) ) ;
#1103 = CARTESIAN_POINT ( 'NONE',  ( 4.270369862968768082, -42.33539640546668892, -99.99920780850642643 ) ) ;
#1104 = DIRECTION ( 'NONE',  ( 1.000000000000000000, 0.000000000000000000, 0.000000000000000000 ) ) ;
#1105 = ADVANCED_FACE ( 'NONE', ( #6898 ), #6943, .T. ) ;
#1106 = FACE_OUTER_BOUND ( 'NONE', #106, .T. ) ;
#1107 = CARTESIAN_POINT ( 'NONE',  ( 4.200000000000001954, 2.694222958124178486E-16, 2.200000000000001066 ) ) ;
#1108 = LINE ( 'NONE', #2483, #4639 ) ;
#1109 = LINE ( 'NONE', #3152, #4900 ) ;
#1110 = CARTESIAN_POINT ( 'NONE',  ( -36.71751442127229836, -42.00000000000000711, -6.717514421272142044 ) ) ;
#1111 =( NAMED_UNIT ( * ) SI_UNIT ( $, .STERADIAN. ) SOLID_ANGLE_UNIT ( ) );
#1112 = ORIENTED_EDGE ( 'NONE', *, *, #3664, .T. ) ;
#1113 = CARTESIAN_POINT ( 'NONE',  ( -38.40363834695740053, -45.69859572486943478, -1.277368040863739118 ) ) ;
#1114 = CARTESIAN_POINT ( 'NONE',  ( -37.06321265474346660, -41.25000000000000711, 7.063212654743582952 ) ) ;
#1115 = CARTESIAN_POINT ( 'NONE',  ( -37.59760657776328685, -43.40140427513058796, 3.811716262761598362 ) ) ;
#1116 = CARTESIAN_POINT ( 'NONE',  ( -1.891708078845683039, -40.43301269999998482, -100.1999999989075292 ) ) ;
#1117 = CARTESIAN_POINT ( 'NONE',  ( -42.00000000000002132, 0.000000000000000000, -28.65000000000000213 ) ) ;
#1118 = CARTESIAN_POINT ( 'NONE',  ( -25.73429323749904185, -40.59859572486944757, -8.488613101951701267 ) ) ;
#1119 = CARTESIAN_POINT ( 'NONE',  ( -37.06321265474346660, -35.24999999999998579, 7.063212654743582952 ) ) ;
#1120 = CARTESIAN_POINT ( 'NONE',  ( -12.65000000000000036, 0.000000000000000000, 0.000000000000000000 ) ) ;
#1121 = CARTESIAN_POINT ( 'NONE',  ( -26.02892847301724544, -48.05549307397419767, 11.85400291056945576 ) ) ;
#1122 = CARTESIAN_POINT ( 'NONE',  ( -1.891708078845683039, -40.43301269999998482, -97.19999999890752918 ) ) ;
#1123 = AXIS2_PLACEMENT_3D ( 'NONE', #1080, #405, #3774 ) ;
#1124 = EDGE_LOOP ( 'NONE', ( #7069, #6657, #3793 ) ) ;
#1125 = ADVANCED_FACE ( 'NONE', ( #203, #4882 ), #244, .F. ) ;
#1126 = CARTESIAN_POINT ( 'NONE',  ( -37.54950433343896776, -48.39859572486944472, 3.906122232810848249 ) ) ;
#1127 = CARTESIAN_POINT ( 'NONE',  ( -20.12537475255788522, -33.05140427513057233, -1.507589171976365439 ) ) ;
#1128 = VERTEX_POINT ( 'NONE', #4173 ) ;
#1129 = CARTESIAN_POINT ( 'NONE',  ( -25.51477047955235378, -33.65140427513057375, 8.925456012876139766 ) ) ;
#1130 = CIRCLE ( 'NONE', #6474, 2.149999999999985256 ) ;
#1131 = DIRECTION ( 'NONE',  ( -0.000000000000000000, 0.000000000000000000, 1.000000000000000000 ) ) ;
#1132 = DIRECTION ( 'NONE',  ( -1.000000000000000000, -0.000000000000000000, -0.000000000000000000 ) ) ;
#1133 = CARTESIAN_POINT ( 'NONE',  ( -4.999999999999998224, -44.99999999999997158, -97.40000000000000568 ) ) ;
#1134 = CARTESIAN_POINT ( 'NONE',  ( 42.00000000000000711, 48.00000000000002842, -20.34999999999992326 ) ) ;
#1135 = CARTESIAN_POINT ( 'NONE',  ( 2.071067811865477282, -49.99999999999996447, -97.15000000000000568 ) ) ;
#1136 = ORIENTED_EDGE ( 'NONE', *, *, #41, .T. ) ;
#1137 = VECTOR ( 'NONE', #1455, 1000.000000000000000 ) ;
#1138 = CARTESIAN_POINT ( 'NONE',  ( -36.31971658582311591, -41.25000000000000711, 6.319716585823199395 ) ) ;
#1139 = PRESENTATION_LAYER_ASSIGNMENT (  '', '', ( #2427 ) ) ;
#1140 = ORIENTED_EDGE ( 'NONE', *, *, #8599, .F. ) ;
#1141 = CARTESIAN_POINT ( 'NONE',  ( 4.999999999999998224, -42.92893218813448897, -98.54999999999999716 ) ) ;
#1142 = DIRECTION ( 'NONE',  ( 0.000000000000000000, 0.000000000000000000, 1.000000000000000000 ) ) ;
#1143 = CARTESIAN_POINT ( 'NONE',  ( -28.72263195913613387, -30.80140427513057233, 8.403638346957361449 ) ) ;
#1144 = CARTESIAN_POINT ( 'NONE',  ( -22.42644454439892598, -39.90000000000000568, -3.858919247786222861 ) ) ;
#1145 = DIRECTION ( 'NONE',  ( 1.000000000000000000, 0.000000000000000000, 0.000000000000000000 ) ) ;
#1146 = FACE_OUTER_BOUND ( 'NONE', #3517, .T. ) ;
#1147 = CARTESIAN_POINT ( 'NONE',  ( -36.31971658582311591, -32.25000000000000711, 6.319716585823200283 ) ) ;
#1148 = EDGE_CURVE ( 'NONE', #1263, #1046, #2502, .T. ) ;
#1149 = CARTESIAN_POINT ( 'NONE',  ( 2.000000000000000000, -0.8865213383406692627, 1.535500000000001641 ) ) ;
#1150 = CARTESIAN_POINT ( 'NONE',  ( -38.90016716647221529, -50.85000000000000142, -4.534861676072185155 ) ) ;
#1151 = DIRECTION ( 'NONE',  ( -1.000000000000000000, 0.000000000000000000, 0.000000000000000000 ) ) ;
#1152 = EDGE_LOOP ( 'NONE', ( #2553, #2380, #260, #2838 ) ) ;
#1153 = CARTESIAN_POINT ( 'NONE',  ( -28.61798213517984024, -44.79859572486943620, 8.387063443159973986 ) ) ;
#1154 = CARTESIAN_POINT ( 'NONE',  ( -25.68709025247441602, -36.60000000000000853, -8.464561979789547053 ) ) ;
#1155 = CIRCLE ( 'NONE', #7353, 1.535500000000000087 ) ;
#1156 = CARTESIAN_POINT ( 'NONE',  ( -21.61293655684001536, -36.20140427513057091, 1.382017864820032971 ) ) ;
#1157 = EDGE_CURVE ( 'NONE', #4571, #3127, #4461, .T. ) ;
#1158 = CARTESIAN_POINT ( 'NONE',  ( -4.566987299999997418, -46.89170807884566017, -98.39999999890753202 ) ) ;
#1159 = LINE ( 'NONE', #7780, #1087 ) ;
#1161 = CARTESIAN_POINT ( 'NONE',  ( -28.49241082802385350, -37.44859572486943478, -9.874625247442173404 ) ) ;
#1160 = AXIS2_PLACEMENT_3D ( 'NONE', #8260, #1369, #7455 ) ;
#1162 = CARTESIAN_POINT ( 'NONE',  ( -37.06321265474346660, -32.25000000000000711, 7.063212654743582952 ) ) ;
#1163 = DIRECTION ( 'NONE',  ( -0.000000000000000000, -0.000000000000000000, 1.000000000000000000 ) ) ;
#1164 = DIRECTION ( 'NONE',  ( -1.000000000000000000, 0.000000000000000000, 0.000000000000000000 ) ) ;
#1165 = CIRCLE ( 'NONE', #5378, 4.999999999999969802 ) ;
#1166 = CARTESIAN_POINT ( 'NONE',  ( -3.229347689422840784, -41.77065231057713390, -95.34999999890753486 ) ) ;
#1167 = ORIENTED_EDGE ( 'NONE', *, *, #3403, .T. ) ;
#1168 = CARTESIAN_POINT ( 'NONE',  ( 44.14999999999999147, 21.99999999999992184, 60.00000000000002842 ) ) ;
#1169 = CARTESIAN_POINT ( 'NONE',  ( -38.81868038277247734, -48.54859572486944330, 1.453139578080855365 ) ) ;
#1170 = CARTESIAN_POINT ( 'NONE',  ( -20.62524821624488069, -33.20140427513057091, 1.538452329860250378 ) ) ;
#1171 = ADVANCED_FACE ( 'NONE', ( #4922 ), #8239, .T. ) ;
#1172 = CIRCLE ( 'NONE', #6516, 10.00000000000000178 ) ;
#1173 = ORIENTED_EDGE ( 'NONE', *, *, #7210, .F. ) ;
#1174 = ORIENTED_EDGE ( 'NONE', *, *, #6666, .F. ) ;
#1175 = CARTESIAN_POINT ( 'NONE',  ( -39.87462524744216807, -37.55140427513057944, 1.507589171976367215 ) ) ;
#1176 = CARTESIAN_POINT ( 'NONE',  ( -34.99999999999997868, -45.33027059730886066, 11.45643923738958847 ) ) ;
#1177 = CARTESIAN_POINT ( 'NONE',  ( -42.00000000000006395, 0.000000000000000000, -29.65000000000000213 ) ) ;
#1178 = ADVANCED_FACE ( 'NONE', ( #5574, #8282 ), #2243, .F. ) ;
#1179 = DIRECTION ( 'NONE',  ( 1.049727191138617093E-16, 0.5150380749100563760, -0.8571673007021110013 ) ) ;
#1180 = CARTESIAN_POINT ( 'NONE',  ( -4.999999999999994671, -47.07106781186546840, -96.55000000000001137 ) ) ;
#1181 = CARTESIAN_POINT ( 'NONE',  ( -2.071067811865475505, -49.99999999999996447, -98.85000000000002274 ) ) ;
#1182 = VECTOR ( 'NONE', #7954, 1000.000000000000000 ) ;
#1183 = ORIENTED_EDGE ( 'NONE', *, *, #2611, .F. ) ;
#1184 = CARTESIAN_POINT ( 'NONE',  ( -36.31971658582311591, -47.25000000000000711, 6.319716585823199395 ) ) ;
#1185 = ORIENTED_EDGE ( 'NONE', *, *, #2970, .F. ) ;
#1186 = CARTESIAN_POINT ( 'NONE',  ( -4.999999999999998224, -44.99999999999997158, -97.40000000000000568 ) ) ;
#1187 = CARTESIAN_POINT ( 'NONE',  ( 30.00000000000001421, -49.99999999999997158, 12.49999999999995914 ) ) ;
#1188 = CARTESIAN_POINT ( 'NONE',  ( -31.45313957808072303, -36.95140427513057801, 8.818680382772479120 ) ) ;
#1189 = EDGE_CURVE ( 'NONE', #5443, #1675, #4966, .T. ) ;
#1190 = CARTESIAN_POINT ( 'NONE',  ( -34.99999999999997868, -45.00000000000000000, 11.45643923738958847 ) ) ;
#1191 = CARTESIAN_POINT ( 'NONE',  ( -36.31971658582311591, -35.25000000000000000, 6.319716585823200283 ) ) ;
#1192 = DIRECTION ( 'NONE',  ( -0.000000000000000000, 1.000000000000000000, 0.000000000000000000 ) ) ;
#1193 = CARTESIAN_POINT ( 'NONE',  ( -21.09983283352783801, -49.35000000000000853, 4.534861676072186043 ) ) ;
#1194 = DIRECTION ( 'NONE',  ( 0.000000000000000000, 0.000000000000000000, 1.000000000000000000 ) ) ;
#1195 = VERTEX_POINT ( 'NONE', #2111 ) ;
#1196 = CARTESIAN_POINT ( 'NONE',  ( -36.28032828410546529, -45.24859572486943904, 6.359104887540839357 ) ) ;
#1197 = CARTESIAN_POINT ( 'NONE',  ( -25.46513832392765408, -37.65000000000000568, 8.900167166472096270 ) ) ;
#1198 = CARTESIAN_POINT ( 'NONE',  ( -37.93801861833426159, -43.85140427513058370, -4.107139971057695682 ) ) ;
#1199 = CIRCLE ( 'NONE', #2764, 1.535500000000000087 ) ;
#1200 = PLANE ( 'NONE',  #368 ) ;
#1201 = DIRECTION ( 'NONE',  ( -0.5150380749100560429, 1.049727191138617340E-16, -0.8571673007021112234 ) ) ;
#1202 = APPLICATION_CONTEXT ( 'automotive_design' ) ;
#1203 = CARTESIAN_POINT ( 'NONE',  ( -38.92545601287626056, -39.84859572486944046, -4.485229520447501450 ) ) ;
#1204 = CARTESIAN_POINT ( 'NONE',  ( -36.71751442127229836, -39.00000000000000711, -6.717514421272142044 ) ) ;
#1205 = LINE ( 'NONE', #5255, #2854 ) ;
#1206 = CARTESIAN_POINT ( 'NONE',  ( 30.00000000000000000, 60.00000000000002842, -1.102182119232617753E-14 ) ) ;
#1207 = CARTESIAN_POINT ( 'NONE',  ( -1.891708078845683039, -40.43301269999998482, -96.19999999890752918 ) ) ;
#1208 = AXIS2_PLACEMENT_3D ( 'NONE', #2158, #8155, #3438 ) ;
#1209 = VERTEX_POINT ( 'NONE', #3102 ) ;
#1210 = DIRECTION ( 'NONE',  ( 0.000000000000000000, 0.5150380749100549327, 0.8571673007021118895 ) ) ;
#1211 = CARTESIAN_POINT ( 'NONE',  ( -21.18131961722757595, -50.04859572486944330, -1.453139578080854699 ) ) ;
#1212 = CARTESIAN_POINT ( 'NONE',  ( -38.90016716647221529, -50.84999999999999432, -4.534861676072185155 ) ) ;
#1213 = ORIENTED_EDGE ( 'NONE', *, *, #4836, .F. ) ;
#1214 = AXIS2_PLACEMENT_3D ( 'NONE', #777, #863, #6858 ) ;
#1215 = ORIENTED_EDGE ( 'NONE', *, *, #8346, .F. ) ;
#1216 = CARTESIAN_POINT ( 'NONE',  ( -39.37475178375516549, -40.70140427513058512, -1.538452329860249712 ) ) ;
#1217 = LINE ( 'NONE', #3913, #4688 ) ;
#1218 = CARTESIAN_POINT ( 'NONE',  ( -24.64110105645932336, 8.000000000000000000, -25.00000000000000000 ) ) ;
#1219 = FACE_OUTER_BOUND ( 'NONE', #2950, .T. ) ;
#1220 = CARTESIAN_POINT ( 'NONE',  ( -4.999999999999998224, -44.99999999999997158, -99.79999999999999716 ) ) ;
#1221 = ORIENTED_EDGE ( 'NONE', *, *, #5114, .F. ) ;
#1222 = CIRCLE ( 'NONE', #3351, 1.535500000000000087 ) ;
#1223 = CARTESIAN_POINT ( 'NONE',  ( -22.42644454439892598, -42.90000000000000568, -3.858919247786222861 ) ) ;
#1224 = AXIS2_PLACEMENT_3D ( 'NONE', #5201, #3231, #6698 ) ;
#1225 = EDGE_LOOP ( 'NONE', ( #7122, #8635, #4534, #6637, #1029, #5348 ) ) ;
#1226 = CYLINDRICAL_SURFACE ( 'NONE', #220, 12.00000000000000000 ) ;
#1227 = CARTESIAN_POINT ( 'NONE',  ( 5.000000000000000000, -47.07106781186545419, -96.25000000000000000 ) ) ;
#1228 = CARTESIAN_POINT ( 'NONE',  ( -20.61696076434619584, -46.20000000000000284, 1.486127417882100676 ) ) ;
#1229 = CARTESIAN_POINT ( 'NONE',  ( 8.389419568037416259E-16, -49.56698729999997255, -98.24999999890752633 ) ) ;
#1230 = DIRECTION ( 'NONE',  ( 0.000000000000000000, -1.000000000000000000, 0.000000000000000000 ) ) ;
#1231 = CARTESIAN_POINT ( 'NONE',  ( -38.38706344316003793, -37.70140427513057091, -1.382017864820032083 ) ) ;
#1232 = ADVANCED_FACE ( 'NONE', ( #5783 ), #2079, .T. ) ;
#1233 = CARTESIAN_POINT ( 'NONE',  ( 2.071067811865477282, -49.99999999999996447, -96.34300000002185982 ) ) ;
#1234 = CARTESIAN_POINT ( 'NONE',  ( -23.98959235991431171, -34.50000000000000000, 6.010407640085604797 ) ) ;
#1235 = CARTESIAN_POINT ( 'NONE',  ( -24.64110105645932336, -8.999999999999998224, -25.00000000000000000 ) ) ;
#1236 = CARTESIAN_POINT ( 'NONE',  ( -49.99999999999997158, -59.99999999999997158, -30.00000000000000000 ) ) ;
#1237 = DIRECTION ( 'NONE',  ( 0.000000000000000000, 1.000000000000000000, 0.000000000000000000 ) ) ;
#1238 = ORIENTED_EDGE ( 'NONE', *, *, #4139, .F. ) ;
#1239 = DIRECTION ( 'NONE',  ( 0.000000000000000000, 1.000000000000000000, -0.000000000000000000 ) ) ;
#1240 = CARTESIAN_POINT ( 'NONE',  ( -21.09983283352784156, -40.35000000000000142, 4.534861676072186043 ) ) ;
#1241 = CARTESIAN_POINT ( 'NONE',  ( -37.93801861833426159, -34.85140427513057659, -4.107139971057695682 ) ) ;
#1242 = CARTESIAN_POINT ( 'NONE',  ( -50.00000000000002842, -44.99999999999997158, 0.000000000000000000 ) ) ;
#1243 = DIRECTION ( 'NONE',  ( -0.000000000000000000, -0.000000000000000000, -1.000000000000000000 ) ) ;
#1244 = CARTESIAN_POINT ( 'NONE',  ( -22.97617564697422665, -37.74859572486943904, -7.102600956461224690 ) ) ;
#1245 = CARTESIAN_POINT ( 'NONE',  ( 2.000000000000000000, 1.773042676681340968, -1.951563910473907981E-15 ) ) ;
#1246 = CARTESIAN_POINT ( 'NONE',  ( 42.00000000000000711, 60.00000000000002842, 21.99999999999992184 ) ) ;
#1247 = CARTESIAN_POINT ( 'NONE',  ( 4.566987299999998307, -44.99999999999997158, -99.04999999890752349 ) ) ;
#1248 = SHAPE_REPRESENTATION_RELATIONSHIP ( 'NONE' , 'NONE' ,  #4396, #24 ) ;
#1249 = VERTEX_POINT ( 'NONE', #2443 ) ;
#1250 = LINE ( 'NONE', #3948, #2876 ) ;
#1251 = CARTESIAN_POINT ( 'NONE',  ( -36.04786814110010340, -48.99859572486944614, -5.972947139071243861 ) ) ;
#1252 = CARTESIAN_POINT ( 'NONE',  ( -28.38237549136062654, -35.45140427513057801, -9.857197362228843573 ) ) ;
#1253 = ORIENTED_EDGE ( 'NONE', *, *, #4029, .F. ) ;
#1254 = ORIENTED_EDGE ( 'NONE', *, *, #636, .T. ) ;
#1255 = CARTESIAN_POINT ( 'NONE',  ( -31.61762450863942320, -45.95140427513058512, 9.857197362228843573 ) ) ;
#1256 = CARTESIAN_POINT ( 'NONE',  ( 11.32499999999999929, 1.386912500034377407E-15, 0.000000000000000000 ) ) ;
#1257 = DIRECTION ( 'NONE',  ( -0.000000000000000000, 1.000000000000000000, -0.000000000000000000 ) ) ;
#1258 = CARTESIAN_POINT ( 'NONE',  ( 4.999999999999998224, -42.92893218813448897, -98.44999999781505551 ) ) ;
#1259 = CARTESIAN_POINT ( 'NONE',  ( -3.535533905932735532, -48.53553390593270933, -98.10000000000000853 ) ) ;
#1260 = ORIENTED_EDGE ( 'NONE', *, *, #4573, .F. ) ;
#1261 = CARTESIAN_POINT ( 'NONE',  ( -31.32969295284206979, -39.30000000000001137, -8.395350895058669494 ) ) ;
#1262 = VECTOR ( 'NONE', #5697, 1000.000000000000000 ) ;
#1263 = VERTEX_POINT ( 'NONE', #6917 ) ;
#1264 = CARTESIAN_POINT ( 'NONE',  ( 3.229347689422839895, -41.77065231057713390, -97.34999999890752065 ) ) ;
#1265 = EDGE_CURVE ( 'NONE', #2617, #8337, #8133, .T. ) ;
#1266 = CARTESIAN_POINT ( 'NONE',  ( -2.071067811865475061, -39.99999999999997158, -99.94999999999998863 ) ) ;
#1267 = CARTESIAN_POINT ( 'NONE',  ( -25.46513832392765408, -46.65000000000001279, 8.900167166472096270 ) ) ;
#1268 = CARTESIAN_POINT ( 'NONE',  ( 3.229347689422841228, -48.22934768942280925, -99.74999999890752633 ) ) ;
#1269 = CARTESIAN_POINT ( 'NONE',  ( 4.766825771567327230, -43.38335435358479941, -100.0003056439282147 ) ) ;
#1270 = CARTESIAN_POINT ( 'NONE',  ( -38.38706344316003793, -34.70140427513057091, -1.382017864820032083 ) ) ;
#1271 = VECTOR ( 'NONE', #2457, 1000.000000000000114 ) ;
#1272 = CARTESIAN_POINT ( 'NONE',  ( -2.071067811865475505, -49.99999999999996447, -96.44300000002185413 ) ) ;
#1273 = CARTESIAN_POINT ( 'NONE',  ( -23.98959235991431171, -37.50000000000000711, 6.010407640085604797 ) ) ;
#1274 = ADVANCED_FACE ( 'NONE', ( #5642 ), #5030, .F. ) ;
#1275 = DIRECTION ( 'NONE',  ( -1.000000000000000000, 0.000000000000000000, 0.000000000000000000 ) ) ;
#1276 = MECHANICAL_DESIGN_GEOMETRIC_PRESENTATION_REPRESENTATION (  '', ( #2556 ), #865 ) ;
#1277 = CARTESIAN_POINT ( 'NONE',  ( -34.31290974752564438, -50.10000000000000853, 8.464561979789547053 ) ) ;
#1278 = ORIENTED_EDGE ( 'NONE', *, *, #3659, .T. ) ;
#1279 = CARTESIAN_POINT ( 'NONE',  ( -24.64110105645932336, 0.000000000000000000, -24.00000000000000000 ) ) ;
#1280 = CARTESIAN_POINT ( 'NONE',  ( -21.53543802021056663, -42.90000000000000568, -4.312909747525783821 ) ) ;
#1281 = CARTESIAN_POINT ( 'NONE',  ( -23.68028341417693738, -30.75000000000000000, -6.319716585823198507 ) ) ;
#1282 = AXIS2_PLACEMENT_3D ( 'NONE', #1511, #4204, #6885 ) ;
#1283 = CARTESIAN_POINT ( 'NONE',  ( -5.000000000000003553, -42.92893218813449607, -96.64999999999999147 ) ) ;
#1284 = DIRECTION ( 'NONE',  ( -0.000000000000000000, -0.000000000000000000, -1.000000000000000000 ) ) ;
#1285 = CARTESIAN_POINT ( 'NONE',  ( -38.44051085762733777, -33.39859572486943762, 4.360112732550414982 ) ) ;
#1286 = LINE ( 'NONE', #4737, #2691 ) ;
#1287 = LINE ( 'NONE', #5256, #1182 ) ;
#1288 = CARTESIAN_POINT ( 'NONE',  ( -4.566987299999998307, -44.99999999999997158, -100.2499999989075121 ) ) ;
#1289 = AXIS2_PLACEMENT_3D ( 'NONE', #4498, #7851, #1977 ) ;
#1290 = ORIENTED_EDGE ( 'NONE', *, *, #3181, .F. ) ;
#1291 = DIRECTION ( 'NONE',  ( 0.000000000000000000, -1.000000000000000000, 0.000000000000000000 ) ) ;
#1292 = CARTESIAN_POINT ( 'NONE',  ( -22.42644454439892598, -45.90000000000001279, -3.858919247786222861 ) ) ;
#1293 =( BOUNDED_CURVE ( )  B_SPLINE_CURVE ( 2, ( #2605, #553, #3265, #272, #8396, #7061, #3021, #2974, #2316, #1023, #4994, #7727, #3715, #7678, #2358, #1641, #6734, #2028, #2121, #7444, #3444, #7356, #4716, #6219, #4098, #7486, #2073, #126, #1402, #3488, #2651, #7400, #4760, #6121, #4143, #4803, #2735, #2825, #1264, #5406, #6775, #693, #8020, #3399, #8064, #78, #4852, #2784, #740, #1355, #2693, #1451, #5449, #8115, #5497, #6689, #8207, #4054, #2166, #8161, #6822, #785, #3965, #6170, #3356, #6642, #599, #6076, #3313, #5987, #34, #8678, #5320, #1980, #4667, #1310, #4010, #647, #6031, #5362, #4184, #6208, #7661, #5586, #6866, #6910, #3003, #4894, #5721, #4227, #2340, #8293, #8250, #6954, #173, #2872, #5544, #8332, #872, #5021, #2209 ),
 .UNSPECIFIED., .F., .T. ) 
 B_SPLINE_CURVE_WITH_KNOTS ( ( 3, 2, 2, 2, 2, 2, 2, 2, 2, 2, 2, 2, 2, 2, 2, 2, 2, 2, 2, 2, 2, 2, 2, 2, 2, 2, 2, 2, 2, 2, 2, 2, 2, 2, 2, 2, 2, 2, 2, 2, 2, 2, 2, 2, 2, 2, 2, 2, 2, 2, 3 ),
 ( 0.000000000000000000, 0.01785714285714285615, 0.03571428571428571230, 0.05357142857142856845, 0.07142857142857142461, 0.08928571428571428770, 0.1071428571428571369, 0.1250000000000000000, 0.1428571428571428492, 0.1607142857142857262, 0.1785714285714285754, 0.1964285714285714246, 0.2142857142857142738, 0.2321428571428571508, 0.2500000000000000000, 0.2678571428571428492, 0.2857142857142856984, 0.3035714285714285476, 0.3214285714285714524, 0.3392857142857143016, 0.3571428571428571508, 0.3750000000000000000, 0.3928571428571428492, 0.4107142857142856984, 0.4285714285714285476, 0.4464285714285714524, 0.4642857142857143016, 0.4821428571428571508, 0.5000000000000000000, 0.5178571428571429047, 0.5357142857142856984, 0.5535714285714286031, 0.5714285714285713969, 0.5892857142857143016, 0.6071428571428570953, 0.6250000000000000000, 0.6428571428571429047, 0.6607142857142856984, 0.6785714285714286031, 0.6964285714285715079, 0.7142857142857143016, 0.7321428571428570953, 0.7500000000000000000, 0.7678571428571429047, 0.7857142857142856984, 0.8035714285714286031, 0.8214285714285713969, 0.8392857142857143016, 0.8571428571428570953, 0.8750000000000000000, 0.8928571428571429047 ),
 .UNSPECIFIED. ) 
 CURVE ( )  GEOMETRIC_REPRESENTATION_ITEM ( )  RATIONAL_B_SPLINE_CURVE ( ( 1.000000000000000000, 0.9238795325112867385, 1.000000000000000000, 0.9238795325112867385, 1.000000000000000000, 0.9238795325112867385, 1.000000000000000000, 0.9238795325112867385, 1.000000000000000000, 0.9238795325112867385, 1.000000000000000000, 0.9238795325112867385, 1.000000000000000000, 0.9238795325112867385, 1.000000000000000000, 0.9238795325112867385, 1.000000000000000000, 0.9238795325112867385, 1.000000000000000000, 0.9238795325112867385, 1.000000000000000000, 0.9238795325112867385, 1.000000000000000000, 0.9238795325112867385, 1.000000000000000000, 0.9238795325112867385, 1.000000000000000000, 0.9238795325112867385, 1.000000000000000000, 0.9238795325112867385, 1.000000000000000000, 0.9238795325112867385, 1.000000000000000000, 0.9238795325112867385, 1.000000000000000000, 0.9238795325112867385, 1.000000000000000000, 0.9238795325112867385, 1.000000000000000000, 0.9238795325112867385, 1.000000000000000000, 0.9238795325112867385, 1.000000000000000000, 0.9238795325112867385, 1.000000000000000000, 0.9238795325112867385, 1.000000000000000000, 0.9238795325112867385, 1.000000000000000000, 0.9238795325112867385, 1.000000000000000000, 0.9238795325112867385, 1.000000000000000000, 0.9238795325112867385, 1.000000000000000000, 0.9238795325112867385, 1.000000000000000000, 0.9238795325112867385, 1.000000000000000000, 0.9238795325112867385, 1.000000000000000000, 0.9238795325112867385, 1.000000000000000000, 0.9238795325112867385, 1.000000000000000000, 0.9238795325112867385, 1.000000000000000000, 0.9238795325112867385, 1.000000000000000000, 0.9238795325112867385, 1.000000000000000000, 0.9238795325112867385, 1.000000000000000000, 0.9238795325112867385, 1.000000000000000000, 0.9238795325112867385, 1.000000000000000000, 0.9238795325112867385, 1.000000000000000000, 0.9238795325112867385, 1.000000000000000000, 0.9238795325112867385, 1.000000000000000000, 0.9238795325112867385, 1.000000000000000000, 0.9238795325112867385, 1.000000000000000000, 0.9238795325112867385, 1.000000000000000000, 0.9238795325112867385, 1.000000000000000000, 0.9238795325112867385, 1.000000000000000000, 0.9238795325112867385, 1.000000000000000000, 0.9238795325112867385, 1.000000000000000000, 0.9238795325112867385, 1.000000000000000000, 0.9238795325112867385, 1.000000000000000000 ) ) 
 REPRESENTATION_ITEM ( '' )  );
#1294 = CARTESIAN_POINT ( 'NONE',  ( -21.07454398712378918, -35.34859572486944046, 4.485229520447505003 ) ) ;
#1295 = CARTESIAN_POINT ( 'NONE',  ( -23.31994607974211675, -42.50140427513057517, 6.754974922286503869 ) ) ;
#1296 = ORIENTED_EDGE ( 'NONE', *, *, #7973, .T. ) ;
#1297 = VERTEX_POINT ( 'NONE', #2924 ) ;
#1298 = CARTESIAN_POINT ( 'NONE',  ( -31.61762450863942320, -42.95140427513058512, 9.857197362228843573 ) ) ;
#1299 = VECTOR ( 'NONE', #459, 1000.000000000000000 ) ;
#1300 =( NAMED_UNIT ( * ) PLANE_ANGLE_UNIT ( ) SI_UNIT ( $, .RADIAN. ) );
#1301 = LINE ( 'NONE', #5396, #2999 ) ;
#1302 = CARTESIAN_POINT ( 'NONE',  ( -3.061616997868382155E-16, -39.99999999999997158, -100.6999999978150555 ) ) ;
#1303 = CARTESIAN_POINT ( 'NONE',  ( 33.97107152698276877, -48.05549307397414793, 11.85400291056944333 ) ) ;
#1304 = CARTESIAN_POINT ( 'NONE',  ( -4.999999999999997335, -47.07106781186546129, -98.95000000000000284 ) ) ;
#1305 = VERTEX_POINT ( 'NONE', #5506 ) ;
#1306 = CARTESIAN_POINT ( 'NONE',  ( -28.67030704715798350, -46.80000000000001137, 8.395350895058669494 ) ) ;
#1307 = DIRECTION ( 'NONE',  ( -1.000000000000000000, -0.000000000000000000, -0.000000000000000000 ) ) ;
#1308 = TOROIDAL_SURFACE ( 'NONE', #7793, 11.32499999999999929, 1.324999999999999956 ) ;
#1309 = LINE ( 'NONE', #7355, #263 ) ;
#1310 = CARTESIAN_POINT ( 'NONE',  ( 1.891708078845685481, -49.56698729999997255, -99.19999999890751496 ) ) ;
#1311 = CARTESIAN_POINT ( 'NONE',  ( -3.535533905932735532, -48.53553390593270933, -97.19999999781504130 ) ) ;
#1312 = CARTESIAN_POINT ( 'NONE',  ( -31.56260684030781505, -46.94999999999998863, 9.865911304835510265 ) ) ;
#1313 = CARTESIAN_POINT ( 'NONE',  ( -1.891708078845683039, -40.43301269999998482, -96.99999999890752633 ) ) ;
#1314 = CARTESIAN_POINT ( 'NONE',  ( 2.000000000000000000, -0.8865213383406692627, 1.535500000000001641 ) ) ;
#1315 = CARTESIAN_POINT ( 'NONE',  ( -28.72263195913613387, -33.80140427513056522, 8.403638346957361449 ) ) ;
#1316 = ADVANCED_FACE ( 'NONE', ( #2172 ), #222, .F. ) ;
#1317 = AXIS2_PLACEMENT_3D ( 'NONE', #1754, #3775, #7828 ) ;
#1318 = CARTESIAN_POINT ( 'NONE',  ( 4.999999999999998224, -42.92893218813448897, -96.94300000002183992 ) ) ;
#1319 = CARTESIAN_POINT ( 'NONE',  ( -36.01040764008574513, -39.00000000000000711, -6.010407640085605685 ) ) ;
#1320 = DIRECTION ( 'NONE',  ( -1.000000000000000000, -0.000000000000000000, -0.000000000000000000 ) ) ;
#1321 = CARTESIAN_POINT ( 'NONE',  ( -34.35889894354067309, 8.000000000000000000, 124.0000000000000000 ) ) ;
#1322 = CARTESIAN_POINT ( 'NONE',  ( -41.99999999999996447, 84.00000000000002842, -22.00000000000000000 ) ) ;
#1323 = ORIENTED_EDGE ( 'NONE', *, *, #1743, .T. ) ;
#1324 = CARTESIAN_POINT ( 'NONE',  ( 30.00000000000000000, 60.00000000000002842, -12.49999999999999467 ) ) ;
#1325 = CARTESIAN_POINT ( 'NONE',  ( -20.13408869516453947, -46.05000000000001137, -1.562606840307983136 ) ) ;
#1326 = CARTESIAN_POINT ( 'NONE',  ( -38.82739432537914581, -32.55000000000000426, 1.398121909749243441 ) ) ;
#1327 = CARTESIAN_POINT ( 'NONE',  ( -26.64110105645932336, -7.999999999999996447, 124.0000000000000000 ) ) ;
#1328 = CARTESIAN_POINT ( 'NONE',  ( 34.00000000000000000, 2.210487472460973191E-16, -1.610000000000000098 ) ) ;
#1329 = CARTESIAN_POINT ( 'NONE',  ( -38.92545601287626056, -42.84859572486944046, -4.485229520447501450 ) ) ;
#1330 = ADVANCED_FACE ( 'NONE', ( #265 ), #489, .F. ) ;
#1331 = CARTESIAN_POINT ( 'NONE',  ( 2.071067811865474173, -39.99999999999997158, -99.14999999781504414 ) ) ;
#1332 = CYLINDRICAL_SURFACE ( 'NONE', #3852, 1.000000000000000888 ) ;
#1333 = CARTESIAN_POINT ( 'NONE',  ( 3.229347689422839895, -41.77065231057713390, -98.94999999890752918 ) ) ;
#1334 =( NAMED_UNIT ( * ) PLANE_ANGLE_UNIT ( ) SI_UNIT ( $, .RADIAN. ) );
#1335 = ORIENTED_EDGE ( 'NONE', *, *, #5477, .T. ) ;
#1336 = DIRECTION ( 'NONE',  ( 0.000000000000000000, 0.000000000000000000, -1.000000000000000000 ) ) ;
#1337 = VECTOR ( 'NONE', #6380, 1000.000000000000000 ) ;
#1338 = CARTESIAN_POINT ( 'NONE',  ( -36.31971658582311591, -47.25000000000000711, 6.319716585823199395 ) ) ;
#1339 = CARTESIAN_POINT ( 'NONE',  ( -20.14280263777121149, -35.04859572486943620, -1.617624508639600833 ) ) ;
#1340 = CARTESIAN_POINT ( 'NONE',  ( -31.61762450863942320, -42.95140427513058512, 9.857197362228843573 ) ) ;
#1341 = ORIENTED_EDGE ( 'NONE', *, *, #2126, .F. ) ;
#1342 = ORIENTED_EDGE ( 'NONE', *, *, #5457, .T. ) ;
#1343 = CARTESIAN_POINT ( 'NONE',  ( -28.56619749409589204, -42.80140427513057944, 9.391326687552490782 ) ) ;
#1344 = SURFACE_SIDE_STYLE ('',( #6065 ) ) ;
#1345 = DIRECTION ( 'NONE',  ( -1.000000000000000000, 0.000000000000000000, 0.000000000000000000 ) ) ;
#1346 = CARTESIAN_POINT ( 'NONE',  ( -3.061616997868382155E-16, -39.99999999999997158, -99.09999999781504698 ) ) ;
#1347 = CARTESIAN_POINT ( 'NONE',  ( -30.00000000000000000, -49.99999999999997158, 12.49999999999997335 ) ) ;
#1348 = CARTESIAN_POINT ( 'NONE',  ( -30.00000000000002842, 0.000000000000000000, -45.00000000000000000 ) ) ;
#1349 =( BOUNDED_CURVE ( )  B_SPLINE_CURVE ( 2, ( #5060, #2339, #8422, #4402, #6463, #3129, #3046, #1847, #7042 ),
 .UNSPECIFIED., .F., .T. ) 
 B_SPLINE_CURVE_WITH_KNOTS ( ( 3, 2, 2, 2, 3 ),
 ( 0.1428571428571428492, 0.1607142857142857262, 0.1785714285714285754, 0.1964285714285714246, 0.2142857142857142738 ),
 .UNSPECIFIED. ) 
 CURVE ( )  GEOMETRIC_REPRESENTATION_ITEM ( )  RATIONAL_B_SPLINE_CURVE ( ( 1.000000000000000000, 0.9238795325112867385, 1.000000000000000000, 0.9238795325112867385, 1.000000000000000000, 0.9238795325112867385, 1.000000000000000000, 0.9238795325112867385, 1.000000000000000000 ) ) 
 REPRESENTATION_ITEM ( '' )  );
#1350 = ORIENTED_EDGE ( 'NONE', *, *, #250, .T. ) ;
#1351 = CARTESIAN_POINT ( 'NONE',  ( -36.31971658582311591, -50.24999999999998579, 6.319716585823199395 ) ) ;
#1352 = CARTESIAN_POINT ( 'NONE',  ( -39.38303923565386100, -35.70000000000000995, -1.486127417882099788 ) ) ;
#1353 = ADVANCED_FACE ( 'NONE', ( #7536 ), #4369, .T. ) ;
#1354 = VERTEX_POINT ( 'NONE', #971 ) ;
#1355 = CARTESIAN_POINT ( 'NONE',  ( -4.566987299999998307, -43.10829192115428299, -97.89999999890751781 ) ) ;
#1356 = CARTESIAN_POINT ( 'NONE',  ( 2.071067811865474173, -39.99999999999997158, -97.54999999781504982 ) ) ;
#1357 = CARTESIAN_POINT ( 'NONE',  ( -25.68709025247441602, -42.60000000000000853, -8.464561979789547053 ) ) ;
#1358 = CARTESIAN_POINT ( 'NONE',  ( -4.566987299999998307, -43.10829192115428299, -96.89999999890751781 ) ) ;
#1359 = DIRECTION ( 'NONE',  ( 0.000000000000000000, -1.000000000000000000, 1.467581828789149532E-15 ) ) ;
#1360 = CARTESIAN_POINT ( 'NONE',  ( -21.16389173201424612, -45.05140427513057944, -1.343104241417630185 ) ) ;
#1361 = VECTOR ( 'NONE', #1439, 1000.000000000000000 ) ;
#1362 = AXIS2_PLACEMENT_3D ( 'NONE', #5707, #8409, #1701 ) ;
#1363 = TOROIDAL_SURFACE ( 'NONE', #5298, 11.32499999999999929, 1.324999999999999956 ) ;
#1364 = CARTESIAN_POINT ( 'NONE',  ( 3.535533905932736420, -41.46446609406723383, -95.29300000002184845 ) ) ;
#1365 = B_SPLINE_CURVE_WITH_KNOTS ( 'NONE', 3,
 ( #100, #6269, #6969, #8177, #4869, #4159, #5558, #4243, #4776, #6926, #3506, #5604, #935, #6183, #2889, #144, #5516, #5425, #8225, #8134, #2093, #4377 ),
 .UNSPECIFIED., .F., .F.,
 ( 4, 2, 2, 2, 2, 2, 2, 2, 2, 2, 4 ),
 ( 0.01579945264986107323, 0.01629290087626467792, 0.01678634910266828609, 0.01777324555547549201, 0.01876014200828270140, 0.01974703846108990732, 0.02073393491389711671, 0.02122738314030071100, 0.02172083136670430875, 0.02270772781951152161, 0.02369462427231873447 ),
 .UNSPECIFIED. ) ;
#1366 = CARTESIAN_POINT ( 'NONE',  ( -31.32969295284206979, -42.30000000000000426, -8.395350895058669494 ) ) ;
#1367 = CARTESIAN_POINT ( 'NONE',  ( 2.000000000000000000, -1.773042676681341634, 2.493664996716660198E-15 ) ) ;
#1368 = ADVANCED_FACE ( 'NONE', ( #3582 ), #5808, .T. ) ;
#1369 = DIRECTION ( 'NONE',  ( 0.000000000000000000, -1.000000000000000000, 0.000000000000000000 ) ) ;
#1370 = APPLICATION_PROTOCOL_DEFINITION ( 'draft international standard', 'automotive_design', 1998, #8148 ) ;
#1371 = ORIENTED_EDGE ( 'NONE', *, *, #3878, .F. ) ;
#1372 = CYLINDRICAL_SURFACE ( 'NONE', #654, 4.999999999999973355 ) ;
#1373 = CARTESIAN_POINT ( 'NONE',  ( -25.68709025247441602, -48.60000000000000142, -8.464561979789547053 ) ) ;
#1374 = CARTESIAN_POINT ( 'NONE',  ( -34.00787565980851213, -47.15140427513058086, -7.988596311142238449 ) ) ;
#1375 = CYLINDRICAL_SURFACE ( 'NONE', #4181, 9.999999999999994671 ) ;
#1376 = CARTESIAN_POINT ( 'NONE',  ( -40.00000000000000000, 1.224646799147353454E-15, 80.00000000000002842 ) ) ;
#1377 = CARTESIAN_POINT ( 'NONE',  ( -22.97617564697422665, -43.74859572486943904, -7.102600956461224690 ) ) ;
#1378 = ADVANCED_FACE ( 'NONE', ( #6728 ), #5228, .F. ) ;
#1379 = CARTESIAN_POINT ( 'NONE',  ( 42.00000000000000711, 48.00000000000002842, 21.99999999999992184 ) ) ;
#1380 = CARTESIAN_POINT ( 'NONE',  ( -39.38303923565386100, -32.70000000000000995, -1.486127417882099788 ) ) ;
#1381 = FILL_AREA_STYLE_COLOUR ( '', #8474 ) ;
#1382 = ORIENTED_EDGE ( 'NONE', *, *, #5368, .F. ) ;
#1383 = CARTESIAN_POINT ( 'NONE',  ( -41.99999999999996447, 22.00000000000000000, 80.00000000000002842 ) ) ;
#1384 = CARTESIAN_POINT ( 'NONE',  ( -31.32969295284206979, -48.30000000000001137, -8.395350895058669494 ) ) ;
#1385 = CARTESIAN_POINT ( 'NONE',  ( -21.55948914237271907, -34.89859572486943762, -4.360112732550413206 ) ) ;
#1386 = CARTESIAN_POINT ( 'NONE',  ( -36.68005392025794009, -38.00140427513057517, -6.754974922286504757 ) ) ;
#1387 = AXIS2_PLACEMENT_3D ( 'NONE', #3825, #5720, #7090 ) ;
#1388 = ORIENTED_EDGE ( 'NONE', *, *, #8346, .T. ) ;
#1389 = EDGE_LOOP ( 'NONE', ( #2321, #2903 ) ) ;
#1390 = CARTESIAN_POINT ( 'NONE',  ( -20.62524821624488069, -42.20140427513058512, 1.538452329860250378 ) ) ;
#1391 = CARTESIAN_POINT ( 'NONE',  ( -25.64110105645932336, 8.000000000000000000, 124.0000000000000000 ) ) ;
#1392 = LINE ( 'NONE', #8630, #8276 ) ;
#1393 = CARTESIAN_POINT ( 'NONE',  ( -2.796473189345805913E-16, -40.43301269999997061, -95.64999999890753202 ) ) ;
#1394 = DIRECTION ( 'NONE',  ( 0.000000000000000000, 0.000000000000000000, -1.000000000000000000 ) ) ;
#1395 = CARTESIAN_POINT ( 'NONE',  ( -35.35889894354067309, 8.000000000000000000, -24.00000000000000000 ) ) ;
#1396 = EDGE_CURVE ( 'NONE', #4453, #4354, #2482, .T. ) ;
#1397 = ORIENTED_EDGE ( 'NONE', *, *, #3272, .F. ) ;
#1398 = CARTESIAN_POINT ( 'NONE',  ( -38.82739432537914581, -50.55000000000001137, 1.398121909749243441 ) ) ;
#1399 = CARTESIAN_POINT ( 'NONE',  ( -22.93678734525658314, -33.75000000000001421, -7.063212654743582952 ) ) ;
#1400 = ORIENTED_EDGE ( 'NONE', *, *, #3769, .F. ) ;
#1401 = EDGE_LOOP ( 'NONE', ( #1260, #6461 ) ) ;
#1402 = CARTESIAN_POINT ( 'NONE',  ( 8.389419568037416259E-16, -49.56698729999997255, -96.84999999890752065 ) ) ;
#1403 = CARTESIAN_POINT ( 'NONE',  ( 2.071067811865477282, -49.99999999999996447, -96.24999999781505267 ) ) ;
#1404 = CARTESIAN_POINT ( 'NONE',  ( -25.68709025247441602, -45.60000000000000853, -8.464561979789547053 ) ) ;
#1405 = CARTESIAN_POINT ( 'NONE',  ( -2.796473189345805913E-16, -40.43301269999997061, -97.84999999890753486 ) ) ;
#1406 = CARTESIAN_POINT ( 'NONE',  ( -31.74999999999995737, 0.000000000000000000, 0.000000000000000000 ) ) ;
#1407 = CARTESIAN_POINT ( 'NONE',  ( -22.40239342223677355, -38.90140427513058086, -3.811716262761597473 ) ) ;
#1408 = AXIS2_PLACEMENT_3D ( 'NONE', #5176, #3731, #6412 ) ;
#1409 = CARTESIAN_POINT ( 'NONE',  ( -3.535533905932735532, -48.53553390593270933, -97.29300000002184845 ) ) ;
#1410 = CARTESIAN_POINT ( 'NONE',  ( -31.32969295284206979, -45.30000000000000426, -8.395350895058669494 ) ) ;
#1411 = CARTESIAN_POINT ( 'NONE',  ( 26.68912794345745709, -48.76061935842967898, 12.05589577412331082 ) ) ;
#1412 = CARTESIAN_POINT ( 'NONE',  ( 42.00000000000000711, 60.00000000000002842, 20.34999999999992326 ) ) ;
#1413 = APPLICATION_PROTOCOL_DEFINITION ( 'draft international standard', 'automotive_design', 1998, #6659 ) ;
#1414 = VECTOR ( 'NONE', #6780, 1000.000000000000000 ) ;
#1415 = VERTEX_POINT ( 'NONE', #2066 ) ;
#1416 = FACE_BOUND ( 'NONE', #1448, .T. ) ;
#1417 = CARTESIAN_POINT ( 'NONE',  ( -23.28248557872775137, -49.50000000000000711, 6.717514421272141156 ) ) ;
#1418 = EDGE_CURVE ( 'NONE', #7457, #2517, #6025, .T. ) ;
#1419 = CARTESIAN_POINT ( 'NONE',  ( -31.45313957808072303, -45.95140427513058512, 8.818680382772479120 ) ) ;
#1420 = CARTESIAN_POINT ( 'NONE',  ( 25.00000000000004619, -44.66998333124461595, 11.45643923738958314 ) ) ;
#1421 = EDGE_CURVE ( 'NONE', #2540, #2072, #5423, .T. ) ;
#1422 = FACE_OUTER_BOUND ( 'NONE', #4365, .T. ) ;
#1423 = CARTESIAN_POINT ( 'NONE',  ( -31.50758917197619979, -50.94859572486944899, 9.874625247442176956 ) ) ;
#1424 = CARTESIAN_POINT ( 'NONE',  ( -4.999999999999998224, -44.99999999999997158, -98.19999999999998863 ) ) ;
#1425 = CARTESIAN_POINT ( 'NONE',  ( -36.71751442127229836, -33.00000000000000711, -6.717514421272142044 ) ) ;
#1426 =( NAMED_UNIT ( * ) PLANE_ANGLE_UNIT ( ) SI_UNIT ( $, .RADIAN. ) );
#1427 = EDGE_LOOP ( 'NONE', ( #3891, #3996 ) ) ;
#1428 = PLANE ( 'NONE',  #6426 ) ;
#1429 = CARTESIAN_POINT ( 'NONE',  ( -38.39535089505872634, -50.70000000000000995, -1.329692952841885267 ) ) ;
#1430 = CARTESIAN_POINT ( 'NONE',  ( -31.50758917197619979, -35.94859572486944188, 9.874625247442176956 ) ) ;
#1431 = CARTESIAN_POINT ( 'NONE',  ( -25.51477047955235378, -39.65140427513058086, 8.925456012876139766 ) ) ;
#1432 =( GEOMETRIC_REPRESENTATION_CONTEXT ( 3 ) GLOBAL_UNCERTAINTY_ASSIGNED_CONTEXT ( ( #5029 ) ) GLOBAL_UNIT_ASSIGNED_CONTEXT ( ( #3763, #3106, #5786 ) ) REPRESENTATION_CONTEXT ( 'NONE', 'WORKASPACE' ) );
#1433 = ADVANCED_FACE ( 'NONE', ( #2687 ), #7405, .F. ) ;
#1434 = VERTEX_POINT ( 'NONE', #549 ) ;
#1435 = ORIENTED_EDGE ( 'NONE', *, *, #5478, .T. ) ;
#1436 = CARTESIAN_POINT ( 'NONE',  ( -4.566987299999998307, -44.99999999999997158, -95.24999999890752633 ) ) ;
#1437 = AXIS2_PLACEMENT_3D ( 'NONE', #3049, #3701, #6381 ) ;
#1438 = VECTOR ( 'NONE', #5779, 1000.000000000000000 ) ;
#1439 = DIRECTION ( 'NONE',  ( -1.000000000000000000, -0.000000000000000000, -0.000000000000000000 ) ) ;
#1440 = CARTESIAN_POINT ( 'NONE',  ( 4.999999999999998224, -42.92893218813448897, -99.24999999781506688 ) ) ;
#1441 = CARTESIAN_POINT ( 'NONE',  ( 4.000000000000003553, 0.000000000000000000, 3.500000000000000000 ) ) ;
#1442 = DIRECTION ( 'NONE',  ( 0.000000000000000000, -0.000000000000000000, 1.000000000000000000 ) ) ;
#1443 = ORIENTED_EDGE ( 'NONE', *, *, #6341, .T. ) ;
#1444 = ADVANCED_FACE ( 'NONE', ( #7394 ), #5354, .F. ) ;
#1445 = CARTESIAN_POINT ( 'NONE',  ( -22.42644454439892598, -48.90000000000000568, -3.858919247786222861 ) ) ;
#1446 = CARTESIAN_POINT ( 'NONE',  ( -28.43739315969223824, -39.45000000000000995, -9.865911304835512041 ) ) ;
#1447 = CIRCLE ( 'NONE', #2579, 1.535500000000000087 ) ;
#1448 = EDGE_LOOP ( 'NONE', ( #7819, #5270 ) ) ;
#1449 = ADVANCED_FACE ( 'NONE', ( #8285 ), #2862, .T. ) ;
#1450 = FACE_OUTER_BOUND ( 'NONE', #5373, .T. ) ;
#1451 = CARTESIAN_POINT ( 'NONE',  ( -1.891708078845683039, -40.43301269999998482, -97.99999999890752633 ) ) ;
#1452 = CARTESIAN_POINT ( 'NONE',  ( -4.999999999999998224, -44.99999999999997158, -98.89999999781504414 ) ) ;
#1453 = CARTESIAN_POINT ( 'NONE',  ( -3.535533905932735532, -48.53553390593270933, -97.99999999781503845 ) ) ;
#1454 = CARTESIAN_POINT ( 'NONE',  ( -4.566987299999998307, -43.10829192115428299, -100.0999999989075349 ) ) ;
#1455 = DIRECTION ( 'NONE',  ( -0.000000000000000000, -0.000000000000000000, -1.000000000000000000 ) ) ;
#1456 = CARTESIAN_POINT ( 'NONE',  ( -28.72263195913613387, -39.80140427513057944, 8.403638346957361449 ) ) ;
#1457 = CARTESIAN_POINT ( 'NONE',  ( 5.000000000000000000, -47.07106781186545419, -95.45000000000000284 ) ) ;
#1458 = CARTESIAN_POINT ( 'NONE',  ( -37.96330746473829976, -44.85000000000000853, -4.057507815433013754 ) ) ;
#1459 = CARTESIAN_POINT ( 'NONE',  ( -2.071067811865475061, -39.99999999999997158, -95.84999999781504698 ) ) ;
#1460 = ORIENTED_EDGE ( 'NONE', *, *, #3286, .T. ) ;
#1461 = DIRECTION ( 'NONE',  ( 0.000000000000000000, 0.000000000000000000, 1.000000000000000000 ) ) ;
#1462 = CARTESIAN_POINT ( 'NONE',  ( -39.38303923565386100, -50.70000000000000995, -1.486127417882099788 ) ) ;
#1463 = CARTESIAN_POINT ( 'NONE',  ( -37.59760657776328685, -49.40140427513058086, 3.811716262761598362 ) ) ;
#1464 = EDGE_CURVE ( 'NONE', #8429, #5042, #3565, .T. ) ;
#1465 = CARTESIAN_POINT ( 'NONE',  ( 27.49109988343930766, -40.67193172067894835, 12.24650812517141674 ) ) ;
#1466 = LINE ( 'NONE', #3507, #6194 ) ;
#1467 = CARTESIAN_POINT ( 'NONE',  ( -21.55948914237271907, -49.89859572486943762, -4.360112732550413206 ) ) ;
#1468 = CARTESIAN_POINT ( 'NONE',  ( 9.184850993605145972E-16, -49.99999999999997158, -98.00000000000000000 ) ) ;
#1469 = CARTESIAN_POINT ( 'NONE',  ( -21.53543802021056663, -33.90000000000000568, -4.312909747525783821 ) ) ;
#1470 = ORIENTED_EDGE ( 'NONE', *, *, #8697, .T. ) ;
#1471 = CARTESIAN_POINT ( 'NONE',  ( -2.071067811865475505, -49.99999999999997158, -98.85000000000003695 ) ) ;
#1472 = ORIENTED_EDGE ( 'NONE', *, *, #6300, .T. ) ;
#1473 = CARTESIAN_POINT ( 'NONE',  ( -36.28032828410546529, -33.24859572486943193, 6.359104887540839357 ) ) ;
#1474 = CARTESIAN_POINT ( 'NONE',  ( -21.55948914237271907, -43.89859572486944472, -4.360112732550413206 ) ) ;
#1475 = CARTESIAN_POINT ( 'NONE',  ( -39.87462524744216807, -37.55140427513057944, 1.507589171976367215 ) ) ;
#1476 = VERTEX_POINT ( 'NONE', #2201 ) ;
#1477 = CARTESIAN_POINT ( 'NONE',  ( -4.566987299999997418, -46.89170807884566017, -95.99999999890752633 ) ) ;
#1478 = CARTESIAN_POINT ( 'NONE',  ( -34.53486167607238144, -30.15000000000000213, -8.900167166472096270 ) ) ;
#1479 = CARTESIAN_POINT ( 'NONE',  ( -32.22066341043710480, -40.51720970344483419, 12.30204028087673862 ) ) ;
#1480 = CARTESIAN_POINT ( 'NONE',  ( 4.566987299999998307, -44.99999999999997158, -97.44999999890751496 ) ) ;
#1481 = CARTESIAN_POINT ( 'NONE',  ( -34.35889894354067309, -7.999999999999996447, 125.0000000000000000 ) ) ;
#1482 = CARTESIAN_POINT ( 'NONE',  ( 0.000000000000000000, -44.99999999999997158, -95.00000000000000000 ) ) ;
#1483 = EDGE_LOOP ( 'NONE', ( #1839, #1601, #3000 ) ) ;
#1484 = CARTESIAN_POINT ( 'NONE',  ( -36.28032828410546529, -36.24859572486943904, 6.359104887540839357 ) ) ;
#1485 = CARTESIAN_POINT ( 'NONE',  ( -22.93678734525658314, -30.75000000000000000, -7.063212654743582952 ) ) ;
#1486 = EDGE_LOOP ( 'NONE', ( #3350, #2470 ) ) ;
#1487 = CARTESIAN_POINT ( 'NONE',  ( -28.51387258211773812, -46.80000000000001137, 9.383039235653802379 ) ) ;
#1488 = CARTESIAN_POINT ( 'NONE',  ( 3.535533905932737309, -48.53553390593270933, -98.59999999781504698 ) ) ;
#1489 = CARTESIAN_POINT ( 'NONE',  ( -30.00000000000002842, 0.000000000000000000, -45.00000000000000000 ) ) ;
#1490 = CARTESIAN_POINT ( 'NONE',  ( 3.535533905932737309, -48.53553390593270933, -100.1999999978150555 ) ) ;
#1491 = DIRECTION ( 'NONE',  ( -1.000000000000000000, -0.000000000000000000, -0.000000000000000000 ) ) ;
#1492 = CARTESIAN_POINT ( 'NONE',  ( -2.796473189345805913E-16, -40.43301269999997061, -97.04999999890752349 ) ) ;
#1493 = CARTESIAN_POINT ( 'NONE',  ( -28.72263195913613387, -42.80140427513057944, 8.403638346957361449 ) ) ;
#1494 = AXIS2_PLACEMENT_3D ( 'NONE', #7551, #1514, #280 ) ;
#1495 = CARTESIAN_POINT ( 'NONE',  ( -4.999999999999998224, -44.99999999999997158, -95.79999999999999716 ) ) ;
#1496 = AXIS2_PLACEMENT_3D ( 'NONE', #3239, #2709, #6749 ) ;
#1497 = CARTESIAN_POINT ( 'NONE',  ( 4.566987299999998307, -44.99999999999997158, -95.64999999890753202 ) ) ;
#1498 = CARTESIAN_POINT ( 'NONE',  ( -31.39812190974910422, -43.95000000000000284, 8.827394325379140483 ) ) ;
#1499 = CARTESIAN_POINT ( 'NONE',  ( -41.99999999999996447, 60.00000000000002842, 20.35000000000000142 ) ) ;
#1500 = ITEM_DEFINED_TRANSFORMATION ( 'NONE', 'NONE', #6353,  #2554 ) ;
#1501 = ORIENTED_EDGE ( 'NONE', *, *, #5685, .F. ) ;
#1502 = CARTESIAN_POINT ( 'NONE',  ( 9.184850993605145972E-16, -49.99999999999997158, -100.2999999978150498 ) ) ;
#1503 = AXIS2_PLACEMENT_3D ( 'NONE', #3408, #7897, #1275 ) ;
#1504 = LINE ( 'NONE', #581, #8365 ) ;
#1505 = CARTESIAN_POINT ( 'NONE',  ( -21.17260567462091458, -40.05000000000001137, -1.398121909749242331 ) ) ;
#1506 = AXIS2_PLACEMENT_3D ( 'NONE', #1715, #5676, #1001 ) ;
#1507 = CARTESIAN_POINT ( 'NONE',  ( 26.02887806073490751, -41.94466314146772845, 11.85397847079113731 ) ) ;
#1508 = AXIS2_PLACEMENT_3D ( 'NONE', #5913, #2660, #8687 ) ;
#1509 = FACE_OUTER_BOUND ( 'NONE', #7442, .T. ) ;
#1510 = CARTESIAN_POINT ( 'NONE',  ( -36.75497492228666374, -45.99859572486943904, -6.680053920257780220 ) ) ;
#1511 = CARTESIAN_POINT ( 'NONE',  ( 0.000000000000000000, -44.99999999999997158, -100.0000000000000000 ) ) ;
#1512 = CARTESIAN_POINT ( 'NONE',  ( -38.46456197978948666, -35.40000000000000568, 4.312909747525784709 ) ) ;
#1513 = ORIENTED_EDGE ( 'NONE', *, *, #3148, .T. ) ;
#1514 = DIRECTION ( 'NONE',  ( 0.000000000000000000, 0.000000000000000000, 1.000000000000000000 ) ) ;
#1515 = ORIENTED_EDGE ( 'NONE', *, *, #137, .F. ) ;
#1516 = CARTESIAN_POINT ( 'NONE',  ( -37.98859631114233792, -42.84859572486944046, -4.007875659808334490 ) ) ;
#1517 = CARTESIAN_POINT ( 'NONE',  ( -31.50758917197619979, -47.94859572486943478, 9.874625247442176956 ) ) ;
#1518 = CARTESIAN_POINT ( 'NONE',  ( -23.31994607974211675, -48.50140427513058938, 6.754974922286503869 ) ) ;
#1519 = ORIENTED_EDGE ( 'NONE', *, *, #1781, .F. ) ;
#1520 = CARTESIAN_POINT ( 'NONE',  ( 1.891708078845685481, -49.56698729999997255, -97.39999999890753202 ) ) ;
#1521 = CARTESIAN_POINT ( 'NONE',  ( -2.071067811865475061, -39.99999999999997158, -99.95000000000000284 ) ) ;
#1522 = DIRECTION ( 'NONE',  ( -1.000000000000000000, 0.000000000000000000, 0.000000000000000000 ) ) ;
#1523 = CARTESIAN_POINT ( 'NONE',  ( 1.891708078845682595, -40.43301269999998482, -97.29999999890750928 ) ) ;
#1524 = DIRECTION ( 'NONE',  ( 0.000000000000000000, 0.000000000000000000, -1.000000000000000000 ) ) ;
#1525 = PLANE ( 'NONE',  #3187 ) ;
#1526 = ORIENTED_EDGE ( 'NONE', *, *, #6608, .F. ) ;
#1527 = CARTESIAN_POINT ( 'NONE',  ( -26.18828373723858149, -31.59859572486943335, -7.597606577763319713 ) ) ;
#1528 = CARTESIAN_POINT ( 'NONE',  ( -36.71751442127229836, -36.00000000000000711, -6.717514421272142044 ) ) ;
#1529 = ORIENTED_EDGE ( 'NONE', *, *, #3755, .F. ) ;
#1530 = CARTESIAN_POINT ( 'NONE',  ( -25.46513832392765408, -43.64999999999999147, 8.900167166472096270 ) ) ;
#1531 = CARTESIAN_POINT ( 'NONE',  ( 42.00000000000000711, 60.00000000000002842, 23.64999999999992042 ) ) ;
#1532 = CARTESIAN_POINT ( 'NONE',  ( -50.00000000000002842, -44.99999999999997158, -2.099999999999997868 ) ) ;
#1533 = LINE ( 'NONE', #4853, #6721 ) ;
#1534 = DIRECTION ( 'NONE',  ( 0.000000000000000000, 0.000000000000000000, -1.000000000000000000 ) ) ;
#1535 = CARTESIAN_POINT ( 'NONE',  ( 4.566987299999998307, -43.10829192115428299, -99.59999999890756328 ) ) ;
#1536 = ADVANCED_FACE ( 'NONE', ( #4843, #4796, #4135, #4219, #5577, #4091, #6201 ), #4925, .F. ) ;
#1537 = ORIENTED_EDGE ( 'NONE', *, *, #4588, .T. ) ;
#1538 = CARTESIAN_POINT ( 'NONE',  ( -33.90612223281073057, -46.10140427513058370, 7.549504333439023718 ) ) ;
#1539 = EDGE_CURVE ( 'NONE', #8159, #6416, #3611, .T. ) ;
#1540 = CARTESIAN_POINT ( 'NONE',  ( -4.999999999999998224, -42.92893218813448897, -99.04300000002184845 ) ) ;
#1541 =( REPRESENTATION_RELATIONSHIP ('NONE','NONE', #2265, #6471 ) REPRESENTATION_RELATIONSHIP_WITH_TRANSFORMATION ( #6393 )SHAPE_REPRESENTATION_RELATIONSHIP( ) );
#1542 = CARTESIAN_POINT ( 'NONE',  ( -4.566987299999998307, -44.99999999999997158, -96.84999999890753486 ) ) ;
#1543 = CARTESIAN_POINT ( 'NONE',  ( -36.31971658582311591, -44.25000000000000000, 6.319716585823200283 ) ) ;
#1544 = AXIS2_PLACEMENT_3D ( 'NONE', #891, #5518, #2182 ) ;
#1545 = CARTESIAN_POINT ( 'NONE',  ( -30.00000000000002842, 0.000000000000000000, -41.34999999999999432 ) ) ;
#1546 = EDGE_CURVE ( 'NONE', #4874, #8668, #2062, .T. ) ;
#1547 = CARTESIAN_POINT ( 'NONE',  ( -31.39812190974910422, -37.94999999999998153, 8.827394325379140483 ) ) ;
#1548 = CIRCLE ( 'NONE', #2830, 1.649999999999998579 ) ;
#1549 = ADVANCED_FACE ( 'NONE', ( #823, #2909, #4176 ), #1525, .F. ) ;
#1550 = DIRECTION ( 'NONE',  ( -0.000000000000000000, -0.000000000000000000, 1.000000000000000000 ) ) ;
#1551 = CARTESIAN_POINT ( 'NONE',  ( 0.000000000000000000, 1.773042676681340968, -1.951563910473907981E-15 ) ) ;
#1552 = CARTESIAN_POINT ( 'NONE',  ( -36.71751442127229836, -33.00000000000000711, -6.717514421272142044 ) ) ;
#1553 = CARTESIAN_POINT ( 'NONE',  ( 3.535533905932737309, -48.53553390593270933, -97.90000000000000568 ) ) ;
#1554 = VECTOR ( 'NONE', #2289, 1000.000000000000000 ) ;
#1555 = DIRECTION ( 'NONE',  ( 0.000000000000000000, 0.000000000000000000, 1.000000000000000000 ) ) ;
#1556 = ORIENTED_EDGE ( 'NONE', *, *, #2461, .F. ) ;
#1557 = CARTESIAN_POINT ( 'NONE',  ( 2.000000000000000000, -0.8865213383406692627, 1.535500000000001641 ) ) ;
#1558 = ORIENTED_EDGE ( 'NONE', *, *, #7155, .F. ) ;
#1559 = CARTESIAN_POINT ( 'NONE',  ( -36.28032828410546529, -36.24859572486943904, 6.359104887540839357 ) ) ;
#1560 = ADVANCED_FACE ( 'NONE', ( #1568 ), #2357, .F. ) ;
#1561 = CARTESIAN_POINT ( 'NONE',  ( -28.49241082802385350, -46.44859572486943478, -9.874625247442173404 ) ) ;
#1562 = CARTESIAN_POINT ( 'NONE',  ( -20.62524821624488069, -48.20140427513058512, 1.538452329860250378 ) ) ;
#1563 = CARTESIAN_POINT ( 'NONE',  ( -3.229347689422839451, -48.22934768942280925, -95.94999999890752918 ) ) ;
#1564 = CARTESIAN_POINT ( 'NONE',  ( -25.46513832392765408, -31.65000000000000568, 8.900167166472096270 ) ) ;
#1565 = CARTESIAN_POINT ( 'NONE',  ( -32.07348704419703012, -40.44729329317338795, 12.32776405682971621 ) ) ;
#1566 = CARTESIAN_POINT ( 'NONE',  ( 8.389419568037416259E-16, -49.56698729999997255, -97.64999999890751781 ) ) ;
#1567 = LINE ( 'NONE', #7478, #7656 ) ;
#1568 = FACE_OUTER_BOUND ( 'NONE', #1483, .T. ) ;
#1569 = ORIENTED_EDGE ( 'NONE', *, *, #6881, .T. ) ;
#1570 = PRODUCT_DEFINITION_FORMATION_WITH_SPECIFIED_SOURCE ( 'ANY', '', #7049, .NOT_KNOWN. ) ;
#1571 = CARTESIAN_POINT ( 'NONE',  ( -22.45049566656107842, -37.89859572486944472, -3.906122232810846917 ) ) ;
#1572 = ADVANCED_FACE ( 'NONE', ( #5537 ), #8242, .T. ) ;
#1573 = CARTESIAN_POINT ( 'NONE',  ( -34.31290974752564438, -44.10000000000000853, 8.464561979789547053 ) ) ;
#1574 = EDGE_CURVE ( 'NONE', #4958, #94, #89, .T. ) ;
#1575 = ORIENTED_EDGE ( 'NONE', *, *, #6921, .F. ) ;
#1576 = PRODUCT_DEFINITION ( 'UNKNOWN', '', #3409, #8552 ) ;
#1577 = CARTESIAN_POINT ( 'NONE',  ( -36.71751442127229836, -51.00000000000000711, -6.717514421272142044 ) ) ;
#1578 = DIRECTION ( 'NONE',  ( 1.000000000000000000, 0.000000000000000000, 0.000000000000000000 ) ) ;
#1579 = CARTESIAN_POINT ( 'NONE',  ( -3.535533905932736864, -41.46446609406723383, -98.19999999781505551 ) ) ;
#1580 = CARTESIAN_POINT ( 'NONE',  ( 3.535533905932736420, -41.46446609406723383, -99.19999999781505551 ) ) ;
#1581 = DIRECTION ( 'NONE',  ( 0.000000000000000000, 0.000000000000000000, 1.000000000000000000 ) ) ;
#1582 = CARTESIAN_POINT ( 'NONE',  ( 1.891708078845685481, -49.56698729999997255, -98.99999999890752633 ) ) ;
#1583 = ORIENTED_EDGE ( 'NONE', *, *, #2646, .F. ) ;
#1584 = CARTESIAN_POINT ( 'NONE',  ( -38.83610826798580717, -49.55140427513056522, 1.343104241417631073 ) ) ;
#1585 = AXIS2_PLACEMENT_3D ( 'NONE', #8295, #1491, #2256 ) ;
#1586 = CARTESIAN_POINT ( 'NONE',  ( 5.000000000000000000, -47.07106781186545419, -99.44300000002183992 ) ) ;
#1587 = AXIS2_PLACEMENT_3D ( 'NONE', #2835, #3455, #8171 ) ;
#1588 = DIRECTION ( 'NONE',  ( 0.000000000000000000, -0.000000000000000000, 1.000000000000000000 ) ) ;
#1589 = CARTESIAN_POINT ( 'NONE',  ( 2.071067811865474173, -39.99999999999997158, -96.74999999781503845 ) ) ;
#1590 = CARTESIAN_POINT ( 'NONE',  ( -33.35889894354067309, -9.999999999999998224, -24.00000000000000000 ) ) ;
#1591 =( NAMED_UNIT ( * ) SI_UNIT ( $, .STERADIAN. ) SOLID_ANGLE_UNIT ( ) );
#1592 = CARTESIAN_POINT ( 'NONE',  ( -34.05750781543318340, -42.15000000000001279, -7.963307464738195840 ) ) ;
#1593 = COLOUR_RGB ( '', 0.72549020, 0.75294118, 0.79215686) ;
#1594 = PRODUCT_DEFINITION_SHAPE ( 'NONE', 'NONE',  #8727 ) ;
#1595 = CYLINDRICAL_SURFACE ( 'NONE', #74, 9.999999999999994671 ) ;
#1596 = DIRECTION ( 'NONE',  ( -0.000000000000000000, -0.000000000000000000, -1.000000000000000000 ) ) ;
#1597 = CARTESIAN_POINT ( 'NONE',  ( -39.86591130483550671, -32.55000000000000426, 1.562606840307984468 ) ) ;
#1598 = VECTOR ( 'NONE', #3859, 1000.000000000000000 ) ;
#1599 = DIRECTION ( 'NONE',  ( -1.000000000000000000, -0.000000000000000000, -0.000000000000000000 ) ) ;
#1600 = CARTESIAN_POINT ( 'NONE',  ( -28.51387258211773812, -43.80000000000000426, 9.383039235653802379 ) ) ;
#1601 = ORIENTED_EDGE ( 'NONE', *, *, #5761, .T. ) ;
#1602 = CARTESIAN_POINT ( 'NONE',  ( 50.00000000000002842, -59.99999999999997158, 30.00000000000000000 ) ) ;
#1603 = B_SPLINE_CURVE_WITH_KNOTS ( 'NONE', 1,
 ( #4353, #6415 ),
 .UNSPECIFIED., .F., .F.,
 ( 2, 2 ),
 ( 0.000000000000000000, 1.000000000000000000 ),
 .UNSPECIFIED. ) ;
#1604 = ORIENTED_EDGE ( 'NONE', *, *, #8180, .F. ) ;
#1605 = CARTESIAN_POINT ( 'NONE',  ( -37.54950433343896776, -36.39859572486944472, 3.906122232810848249 ) ) ;
#1606 = CARTESIAN_POINT ( 'NONE',  ( -25.73429323749904185, -46.59859572486944046, -8.488613101951701267 ) ) ;
#1607 = CARTESIAN_POINT ( 'NONE',  ( -34.48522952044771017, -47.15140427513058086, -8.925456012876139766 ) ) ;
#1608 = AXIS2_PLACEMENT_3D ( 'NONE', #2572, #5245, #8717 ) ;
#1609 = EDGE_CURVE ( 'NONE', #3466, #3121, #6430, .T. ) ;
#1610 = CARTESIAN_POINT ( 'NONE',  ( -4.566987299999998307, -44.99999999999997158, -97.64999999890753202 ) ) ;
#1611 = SURFACE_STYLE_USAGE ( .BOTH. , #3519 ) ;
#1612 = CARTESIAN_POINT ( 'NONE',  ( -30.00000000000023093, 0.000000000000000000, -44.00000000000000000 ) ) ;
#1613 = CARTESIAN_POINT ( 'NONE',  ( -1.891708078845683039, -40.43301269999998482, -97.19999999890752918 ) ) ;
#1614 = CARTESIAN_POINT ( 'NONE',  ( -26.94596629111760322, -48.97208017019580950, 12.12430375744701827 ) ) ;
#1615 = CARTESIAN_POINT ( 'NONE',  ( -1.891708078845683039, -40.43301269999998482, -95.59999999890753486 ) ) ;
#1616 = DIRECTION ( 'NONE',  ( 0.000000000000000000, 0.000000000000000000, 1.000000000000000000 ) ) ;
#1617 = VERTEX_POINT ( 'NONE', #5442 ) ;
#1618 = CARTESIAN_POINT ( 'NONE',  ( -26.18828373723858149, -40.59859572486944757, -7.597606577763319713 ) ) ;
#1619 = CARTESIAN_POINT ( 'NONE',  ( -23.28248557872775137, -46.50000000000000711, 6.717514421272141156 ) ) ;
#1620 = ORIENTED_EDGE ( 'NONE', *, *, #6650, .T. ) ;
#1621 = CARTESIAN_POINT ( 'NONE',  ( -20.13408869516453947, -49.04999999999999716, -1.562606840307983136 ) ) ;
#1622 = DIRECTION ( 'NONE',  ( -0.000000000000000000, 1.000000000000000000, -0.000000000000000000 ) ) ;
#1623 = FACE_OUTER_BOUND ( 'NONE', #5831, .T. ) ;
#1624 = CARTESIAN_POINT ( 'NONE',  ( -3.535533905932736864, -41.46446609406723383, -98.99999999781503845 ) ) ;
#1625 = CARTESIAN_POINT ( 'NONE',  ( -30.00000000000000000, 60.00000000000002842, -12.49999999999998934 ) ) ;
#1626 = CARTESIAN_POINT ( 'NONE',  ( -3.229347689422840784, -41.77065231057713390, -97.74999999890752633 ) ) ;
#1627 = ORIENTED_EDGE ( 'NONE', *, *, #6127, .F. ) ;
#1628 = PRODUCT ( 'socket head cap screw_iso_ISO 4762 M4 x 30 - 20N', 'socket head cap screw_iso_ISO 4762 M4 x 30 - 20N', '', ( #5555 ) ) ;
#1629 = CARTESIAN_POINT ( 'NONE',  ( -26.14108075221394856, -33.60000000000000142, -7.573555455601170827 ) ) ;
#1630 = EDGE_CURVE ( 'NONE', #5319, #6677, #8611, .T. ) ;
#1631 = AXIS2_PLACEMENT_3D ( 'NONE', #6294, #255, #418 ) ;
#1632 = CARTESIAN_POINT ( 'NONE',  ( -4.999999999999997335, -47.07106781186546129, -99.74300000002186550 ) ) ;
#1633 = DIRECTION ( 'NONE',  ( 0.000000000000000000, 0.000000000000000000, 1.000000000000000000 ) ) ;
#1634 = CARTESIAN_POINT ( 'NONE',  ( 9.184850993605145972E-16, -49.99999999999997158, -97.09999999781504698 ) ) ;
#1635 = VECTOR ( 'NONE', #5981, 1000.000000000000000 ) ;
#1636 = CARTESIAN_POINT ( 'NONE',  ( 30.00000000000000000, -49.99999999999997158, -12.49999999999998046 ) ) ;
#1637 =( BOUNDED_CURVE ( )  B_SPLINE_CURVE ( 2, ( #3372, #1283, #7418, #8568, #3983, #6004, #7283, #4733, #7376 ),
 .UNSPECIFIED., .F., .T. ) 
 B_SPLINE_CURVE_WITH_KNOTS ( ( 3, 2, 2, 2, 3 ),
 ( 0.2857142857142856429, 0.3035714285714284921, 0.3214285714285713969, 0.3392857142857142461, 0.3571428571428570953 ),
 .UNSPECIFIED. ) 
 CURVE ( )  GEOMETRIC_REPRESENTATION_ITEM ( )  RATIONAL_B_SPLINE_CURVE ( ( 1.000000000000000222, 0.9238795325112865164, 1.000000000000000000, 0.9238795325112867385, 1.000000000000000000, 0.9238795325112867385, 1.000000000000000000, 0.9238795325112869605, 0.9999999999999997780 ) ) 
 REPRESENTATION_ITEM ( '' )  );
#1638 = AXIS2_PLACEMENT_3D ( 'NONE', #235, #8314, #8308 ) ;
#1639 = CARTESIAN_POINT ( 'NONE',  ( -4.999999999999998224, -42.92893218813449607, -100.5499999978150498 ) ) ;
#1640 = CARTESIAN_POINT ( 'NONE',  ( -38.82739432537914581, -41.55000000000001137, 1.398121909749243441 ) ) ;
#1641 = CARTESIAN_POINT ( 'NONE',  ( -4.566987299999997418, -46.89170807884566017, -96.19999999890751496 ) ) ;
#1642 = EDGE_CURVE ( 'NONE', #3619, #6952, #5026, .T. ) ;
#1643 = DIRECTION ( 'NONE',  ( -0.000000000000000000, 1.000000000000000000, -0.000000000000000000 ) ) ;
#1644 = CARTESIAN_POINT ( 'NONE',  ( -25.68709025247441602, -30.60000000000000142, -8.464561979789547053 ) ) ;
#1645 = DIRECTION ( 'NONE',  ( 1.000000000000000000, 0.000000000000000000, 0.000000000000000000 ) ) ;
#1646 = CARTESIAN_POINT ( 'NONE',  ( -34.53486167607238855, -45.15000000000000568, -8.900167166472096270 ) ) ;
#1647 = CIRCLE ( 'NONE', #6298, 1.000000000000000888 ) ;
#1648 = ORIENTED_EDGE ( 'NONE', *, *, #803, .T. ) ;
#1649 = DIRECTION ( 'NONE',  ( -0.7061138087190628188, 0.05297714858780522285, 0.7061138087190791390 ) ) ;
#1650 = ORIENTED_EDGE ( 'NONE', *, *, #3971, .T. ) ;
#1651 = CARTESIAN_POINT ( 'NONE',  ( -23.71967171589458445, -34.74859572486943904, -6.359104887540838469 ) ) ;
#1652 = CARTESIAN_POINT ( 'NONE',  ( -21.07454398712378918, -50.34859572486944046, 4.485229520447505003 ) ) ;
#1653 = CARTESIAN_POINT ( 'NONE',  ( -26.09387776718931917, -32.60140427513057659, -7.549504333439021941 ) ) ;
#1654 = VECTOR ( 'NONE', #2362, 1000.000000000000000 ) ;
#1655 = ADVANCED_FACE ( 'NONE', ( #119 ), #1066, .T. ) ;
#1656 = CARTESIAN_POINT ( 'NONE',  ( 1.891708078845682595, -40.43301269999998482, -99.49999999890752633 ) ) ;
#1657 = CARTESIAN_POINT ( 'NONE',  ( 25.03240331249625328, -45.65721116879221597, 11.47074269425085191 ) ) ;
#1658 =( NAMED_UNIT ( * ) PLANE_ANGLE_UNIT ( ) SI_UNIT ( $, .RADIAN. ) );
#1659 = CARTESIAN_POINT ( 'NONE',  ( -4.566987299999998307, -43.10829192115428299, -97.09999999890752065 ) ) ;
#1660 = CARTESIAN_POINT ( 'NONE',  ( -26.64110105645932336, -7.999999999999996447, 124.0000000000000000 ) ) ;
#1661 = CARTESIAN_POINT ( 'NONE',  ( -2.796473189345805913E-16, -40.43301269999997061, -96.44999999890751496 ) ) ;
#1662 = CARTESIAN_POINT ( 'NONE',  ( 2.000000000000000000, 0.000000000000000000, 1.535500000000000087 ) ) ;
#1663 = VERTEX_POINT ( 'NONE', #859 ) ;
#1664 = CARTESIAN_POINT ( 'NONE',  ( -33.81171626276147890, -39.09859572486944046, 7.597606577763319713 ) ) ;
#1665 = CARTESIAN_POINT ( 'NONE',  ( -38.90016716647221529, -44.85000000000001563, -4.534861676072185155 ) ) ;
#1666 =( REPRESENTATION_RELATIONSHIP ('NONE','NONE', #2265, #7097 ) REPRESENTATION_RELATIONSHIP_WITH_TRANSFORMATION ( #7584 )SHAPE_REPRESENTATION_RELATIONSHIP( ) );
#1667 = ORIENTED_EDGE ( 'NONE', *, *, #1064, .T. ) ;
#1668 = CARTESIAN_POINT ( 'NONE',  ( -38.46456197978948666, -44.40000000000000568, 4.312909747525784709 ) ) ;
#1669 = CARTESIAN_POINT ( 'NONE',  ( -32.51667136668694269, -49.33273298888241243, 12.24717930254582043 ) ) ;
#1670 = CARTESIAN_POINT ( 'NONE',  ( -3.061616997868382155E-16, -39.99999999999997158, -98.29999999781504982 ) ) ;
#1671 = EDGE_CURVE ( 'NONE', #2194, #2812, #4622, .T. ) ;
#1672 = CARTESIAN_POINT ( 'NONE',  ( 42.00000000000000711, 60.00000000000002842, -21.99999999999992184 ) ) ;
#1673 = CARTESIAN_POINT ( 'NONE',  ( 30.00000000000000000, 60.00000000000002842, -12.49999999999998757 ) ) ;
#1674 = CARTESIAN_POINT ( 'NONE',  ( 3.535533905932736420, -41.46446609406723383, -95.29999999999999716 ) ) ;
#1675 = VERTEX_POINT ( 'NONE', #6365 ) ;
#1676 = CARTESIAN_POINT ( 'NONE',  ( -31.32969295284206979, -30.30000000000000782, -8.395350895058669494 ) ) ;
#1677 = EDGE_LOOP ( 'NONE', ( #5190, #1290, #7369, #3341, #3312, #2576 ) ) ;
#1678 = UNCERTAINTY_MEASURE_WITH_UNIT (LENGTH_MEASURE( 1.000000000000000082E-05 ), #6656, 'distance_accuracy_value', 'NONE');
#1679 = DIRECTION ( 'NONE',  ( 0.000000000000000000, 0.000000000000000000, 1.000000000000000000 ) ) ;
#1680 = DIRECTION ( 'NONE',  ( -1.000000000000000000, -0.000000000000000000, -0.000000000000000000 ) ) ;
#1681 = LINE ( 'NONE', #6437, #4511 ) ;
#1682 = ITEM_DEFINED_TRANSFORMATION ( 'NONE', 'NONE', #5098,  #2554 ) ;
#1683 = CARTESIAN_POINT ( 'NONE',  ( -4.999999999999998224, -44.99999999999997158, -98.09999999781504698 ) ) ;
#1684 = CARTESIAN_POINT ( 'NONE',  ( -22.03669253526174998, -40.35000000000000142, 4.057507815433014642 ) ) ;
#1685 = CARTESIAN_POINT ( 'NONE',  ( -50.00000000000002842, -30.00000000000000000, 60.00000000000002842 ) ) ;
#1686 = VECTOR ( 'NONE', #3151, 1000.000000000000000 ) ;
#1687 =( BOUNDED_CURVE ( )  B_SPLINE_CURVE ( 2, ( #3530, #8249, #1488, #4142, #6207, #172, #918, #3613, #5496 ),
 .UNSPECIFIED., .F., .T. ) 
 B_SPLINE_CURVE_WITH_KNOTS ( ( 3, 2, 2, 2, 3 ),
 ( 0.4999999999999999445, 0.5178571428571429047, 0.5357142857142856984, 0.5535714285714286031, 0.5714285714285713969 ),
 .UNSPECIFIED. ) 
 CURVE ( )  GEOMETRIC_REPRESENTATION_ITEM ( )  RATIONAL_B_SPLINE_CURVE ( ( 1.000000000000000222, 0.9238795325112865164, 1.000000000000000000, 0.9238795325112867385, 1.000000000000000000, 0.9238795325112867385, 1.000000000000000000, 0.9238795325112867385, 1.000000000000000000 ) ) 
 REPRESENTATION_ITEM ( '' )  );
#1688 = CARTESIAN_POINT ( 'NONE',  ( 42.00000000000000711, 60.00000000000002842, -20.34999999999992326 ) ) ;
#1689 = CARTESIAN_POINT ( 'NONE',  ( -38.46456197978948666, -35.40000000000000568, 4.312909747525784709 ) ) ;
#1690 = CARTESIAN_POINT ( 'NONE',  ( -41.99999999999981526, 0.000000000000000000, -44.00000000000000000 ) ) ;
#1691 = CARTESIAN_POINT ( 'NONE',  ( -39.38303923565386100, -41.70000000000000995, -1.486127417882099788 ) ) ;
#1692 = EDGE_CURVE ( 'NONE', #6529, #4035, #5048, .T. ) ;
#1693 = SURFACE_STYLE_FILL_AREA ( #7773 ) ;
#1694 = ORIENTED_EDGE ( 'NONE', *, *, #3020, .F. ) ;
#1695 = VERTEX_POINT ( 'NONE', #5090 ) ;
#1696 = CARTESIAN_POINT ( 'NONE',  ( -28.65689575858256077, -37.44859572486943478, -8.836108267985801845 ) ) ;
#1697 = CARTESIAN_POINT ( 'NONE',  ( -34.26570676250101855, -48.09859572486944046, 8.488613101951703044 ) ) ;
#1698 = CARTESIAN_POINT ( 'NONE',  ( -25.99212434019154472, -30.65140427513057730, 7.988596311142242890 ) ) ;
#1699 = VECTOR ( 'NONE', #4425, 1000.000000000000000 ) ;
#1700 = DIRECTION ( 'NONE',  ( -0.000000000000000000, 1.000000000000000000, -0.000000000000000000 ) ) ;
#1701 = DIRECTION ( 'NONE',  ( 1.000000000000000000, 0.000000000000000000, 0.000000000000000000 ) ) ;
#1702 = CARTESIAN_POINT ( 'NONE',  ( -34.31290974752564438, -41.10000000000000142, 8.464561979789547053 ) ) ;
#1703 = PRODUCT_DEFINITION_SHAPE ( 'NONE', 'NONE',  #2226 ) ;
#1704 = CARTESIAN_POINT ( 'NONE',  ( -1.891708078845683039, -40.43301269999998482, -100.3999999989075178 ) ) ;
#1705 = CARTESIAN_POINT ( 'NONE',  ( -30.00000000000000000, -49.99999999999997158, 12.49999999999997335 ) ) ;
#1706 = CARTESIAN_POINT ( 'NONE',  ( -4.566987299999998307, -44.99999999999997158, -95.44999999890751496 ) ) ;
#1707 = DIRECTION ( 'NONE',  ( 0.000000000000000000, 0.000000000000000000, 1.000000000000000000 ) ) ;
#1708 = ORIENTED_EDGE ( 'NONE', *, *, #1546, .F. ) ;
#1709 = EDGE_CURVE ( 'NONE', #6150, #799, #7076, .T. ) ;
#1710 = CARTESIAN_POINT ( 'NONE',  ( -33.81171626276147890, -45.09859572486944046, 7.597606577763319713 ) ) ;
#1711 = CARTESIAN_POINT ( 'NONE',  ( -21.53543802021056663, -45.90000000000001279, -4.312909747525783821 ) ) ;
#1712 = AXIS2_PLACEMENT_3D ( 'NONE', #6266, #5601, #7672 ) ;
#1713 = VERTEX_POINT ( 'NONE', #8449 ) ;
#1714 = CARTESIAN_POINT ( 'NONE',  ( -37.10260095646111012, -31.25140427513058228, 7.023824353025939438 ) ) ;
#1715 = CARTESIAN_POINT ( 'NONE',  ( -41.99999999999996447, 22.00000000000000000, 80.00000000000002842 ) ) ;
#1716 = DIRECTION ( 'NONE',  ( -0.000000000000000000, 1.000000000000000000, -0.000000000000000000 ) ) ;
#1717 = CARTESIAN_POINT ( 'NONE',  ( 2.071067811865474173, -39.99999999999997158, -97.54999999781504982 ) ) ;
#1718 = STYLED_ITEM ( 'NONE', ( #4912 ), #3705 ) ;
#1719 = DIRECTION ( 'NONE',  ( -1.000000000000000000, 0.000000000000000000, 0.000000000000000000 ) ) ;
#1720 = CARTESIAN_POINT ( 'NONE',  ( 9.184850993605145972E-16, -49.99999999999997158, -98.00000000000000000 ) ) ;
#1721 = ORIENTED_EDGE ( 'NONE', *, *, #1642, .T. ) ;
#1722 = CARTESIAN_POINT ( 'NONE',  ( -38.39535089505872634, -35.70000000000000995, -1.329692952841885267 ) ) ;
#1723 = EDGE_CURVE ( 'NONE', #1046, #5443, #2412, .T. ) ;
#1724 = PRODUCT_DEFINITION_FORMATION_WITH_SPECIFIED_SOURCE ( 'ANY', '', #1062, .NOT_KNOWN. ) ;
#1725 = ORIENTED_EDGE ( 'NONE', *, *, #7252, .T. ) ;
#1726 = EDGE_CURVE ( 'NONE', #7832, #2418, #732, .T. ) ;
#1728 = CARTESIAN_POINT ( 'NONE',  ( 5.000000000000000000, -47.07106781186545419, -97.04999999999999716 ) ) ;
#1727 = CIRCLE ( 'NONE', #8211, 1.649999999999998579 ) ;
#1729 = CARTESIAN_POINT ( 'NONE',  ( -3.535533905932736864, -41.46446609406723383, -97.39999999781504414 ) ) ;
#1730 = AXIS2_PLACEMENT_3D ( 'NONE', #3712, #5159, #5825 ) ;
#1731 = FACE_BOUND ( 'NONE', #6833, .T. ) ;
#1732 = DIRECTION ( 'NONE',  ( -1.000000000000000000, 0.000000000000000000, 0.000000000000000000 ) ) ;
#1733 = CARTESIAN_POINT ( 'NONE',  ( -36.01040764008574513, -45.00000000000000711, -6.010407640085605685 ) ) ;
#1734 = CIRCLE ( 'NONE', #7079, 1.535500000000000087 ) ;
#1735 = VECTOR ( 'NONE', #3213, 1000.000000000000000 ) ;
#1736 = DIRECTION ( 'NONE',  ( -0.000000000000000000, 0.000000000000000000, 1.000000000000000000 ) ) ;
#1737 = DIRECTION ( 'NONE',  ( 1.000000000000000000, 0.000000000000000000, 0.000000000000000000 ) ) ;
#1738 = FACE_OUTER_BOUND ( 'NONE', #5933, .T. ) ;
#1739 = CARTESIAN_POINT ( 'NONE',  ( -38.46456197978948666, -38.40000000000000568, 4.312909747525784709 ) ) ;
#1740 = CARTESIAN_POINT ( 'NONE',  ( -49.99999999999997158, 60.00000000000002842, 30.00000000000000000 ) ) ;
#1741 = CARTESIAN_POINT ( 'NONE',  ( -31.56260684030781505, -40.95000000000000995, 9.865911304835508489 ) ) ;
#1742 = PRESENTATION_STYLE_ASSIGNMENT (( #8356 ) ) ;
#1743 = EDGE_CURVE ( 'NONE', #2012, #2194, #4557, .T. ) ;
#1744 = VECTOR ( 'NONE', #7293, 1000.000000000000000 ) ;
#1745 = ORIENTED_EDGE ( 'NONE', *, *, #41, .F. ) ;
#1746 = CARTESIAN_POINT ( 'NONE',  ( -25.89286002894218086, -47.64859572486945183, 7.938018618334153231 ) ) ;
#1747 = CARTESIAN_POINT ( 'NONE',  ( -20.61696076434619584, -34.20000000000000995, 1.486127417882100676 ) ) ;
#1748 = CARTESIAN_POINT ( 'NONE',  ( -35.97294713907137975, -41.00140427513057517, -6.047868141099968398 ) ) ;
#1749 = CARTESIAN_POINT ( 'NONE',  ( -3.229347689422840784, -41.77065231057713390, -100.1499999989075320 ) ) ;
#1750 = UNCERTAINTY_MEASURE_WITH_UNIT (LENGTH_MEASURE( 1.000000000000000082E-05 ), #6287, 'distance_accuracy_value', 'NONE');
#1751 = DIRECTION ( 'NONE',  ( -1.224646799147353207E-16, 1.000000000000000000, 0.000000000000000000 ) ) ;
#1752 = CARTESIAN_POINT ( 'NONE',  ( -38.90016716647221529, -32.85000000000000853, -4.534861676072185155 ) ) ;
#1753 = DIRECTION ( 'NONE',  ( 1.000000000000000000, 0.000000000000000000, 0.000000000000000000 ) ) ;
#1754 = CARTESIAN_POINT ( 'NONE',  ( -50.00000000000002842, -44.99999999999997158, 0.000000000000000000 ) ) ;
#1755 = CARTESIAN_POINT ( 'NONE',  ( -1.891708078845683483, -49.56698729999997255, -96.89999999890751781 ) ) ;
#1756 = FACE_OUTER_BOUND ( 'NONE', #2107, .T. ) ;
#1757 = ORIENTED_EDGE ( 'NONE', *, *, #818, .F. ) ;
#1758 = CARTESIAN_POINT ( 'NONE',  ( -23.95213185889994989, -44.49859572486944614, 5.972947139071243861 ) ) ;
#1759 = VECTOR ( 'NONE', #5840, 1000.000000000000000 ) ;
#1760 = CARTESIAN_POINT ( 'NONE',  ( -20.13408869516453947, -43.04999999999999005, -1.562606840307983136 ) ) ;
#1761 = ORIENTED_EDGE ( 'NONE', *, *, #5886, .T. ) ;
#1762 = CARTESIAN_POINT ( 'NONE',  ( -38.87487832006816291, -34.85140427513057659, -4.584493831696867971 ) ) ;
#1763 = DIRECTION ( 'NONE',  ( -0.000000000000000000, -0.000000000000000000, -1.000000000000000000 ) ) ;
#1764 = CARTESIAN_POINT ( 'NONE',  ( -30.00000000000002487, 0.000000000000000000, -41.35000000000000142 ) ) ;
#1765 = CARTESIAN_POINT ( 'NONE',  ( -4.999999999999998224, -42.92893218813449607, -97.34999999781506119 ) ) ;
#1766 = EDGE_CURVE ( 'NONE', #5152, #5525, #1637, .T. ) ;
#1767 = DIRECTION ( 'NONE',  ( -0.000000000000000000, -0.000000000000000000, -1.000000000000000000 ) ) ;
#1768 = CARTESIAN_POINT ( 'NONE',  ( -2.071067811865475505, -49.99999999999996447, -96.45000000000000284 ) ) ;
#1769 = ORIENTED_EDGE ( 'NONE', *, *, #2902, .T. ) ;
#1770 = CARTESIAN_POINT ( 'NONE',  ( -23.68028341417693738, -36.75000000000000711, -6.319716585823198507 ) ) ;
#1771 = ORIENTED_EDGE ( 'NONE', *, *, #3148, .F. ) ;
#1772 = PRODUCT_DEFINITION_CONTEXT ( 'detailed design', #8148, 'design' ) ;
#1773 = CARTESIAN_POINT ( 'NONE',  ( -4.999999999999998224, -42.92893218813448897, -99.05000000000001137 ) ) ;
#1774 = CARTESIAN_POINT ( 'NONE',  ( -3.535533905932735532, -48.53553390593270933, -96.39999999781505835 ) ) ;
#1775 = DIRECTION ( 'NONE',  ( 1.000000000000000000, 0.000000000000000000, -0.000000000000000000 ) ) ;
#1776 = AXIS2_PLACEMENT_3D ( 'NONE', #4486, #5186, #6424 ) ;
#1777 = CONTEXT_DEPENDENT_SHAPE_REPRESENTATION ( #1098, #3645 ) ;
#1778 = LINE ( 'NONE', #4007, #5943 ) ;
#1779 = CARTESIAN_POINT ( 'NONE',  ( -30.00000000000002487, 0.000000000000000000, -28.65000000000000213 ) ) ;
#1780 = CARTESIAN_POINT ( 'NONE',  ( 42.00000000000000711, -21.99999999999992184, 80.00000000000002842 ) ) ;
#1781 = EDGE_CURVE ( 'NONE', #5443, #3221, #5287, .T. ) ;
#1782 = DIRECTION ( 'NONE',  ( 1.000000000000000000, 0.000000000000000000, 0.000000000000000000 ) ) ;
#1783 = CARTESIAN_POINT ( 'NONE',  ( -34.53486167607238855, -39.14999999999999858, -8.900167166472096270 ) ) ;
#1784 = VERTEX_POINT ( 'NONE', #711 ) ;
#1785 = CARTESIAN_POINT ( 'NONE',  ( -36.75497492228666374, -30.99859572486944259, -6.680053920257780220 ) ) ;
#1786 = CARTESIAN_POINT ( 'NONE',  ( -39.86591130483550671, -32.55000000000000426, 1.562606840307984468 ) ) ;
#1787 = CARTESIAN_POINT ( 'NONE',  ( -28.72263195913613387, -42.80140427513057944, 8.403638346957361449 ) ) ;
#1788 = AXIS2_PLACEMENT_3D ( 'NONE', #4252, #2234, #6318 ) ;
#1789 = CARTESIAN_POINT ( 'NONE',  ( -1.891708078845683705, -49.56698729999997255, -98.29999999890752349 ) ) ;
#1790 = CARTESIAN_POINT ( 'NONE',  ( 2.000000000000000000, 0.8865213383406683745, -1.535500000000000753 ) ) ;
#1791 = CARTESIAN_POINT ( 'NONE',  ( -28.43739315969223824, -36.45000000000000284, -9.865911304835512041 ) ) ;
#1792 = CARTESIAN_POINT ( 'NONE',  ( -3.229347689422840784, -41.77065231057713390, -100.3499999989075206 ) ) ;
#1793 = FACE_OUTER_BOUND ( 'NONE', #1083, .T. ) ;
#1794 = CARTESIAN_POINT ( 'NONE',  ( -4.566987299999997418, -46.89170807884566727, -97.79999999890752349 ) ) ;
#1795 = VERTEX_POINT ( 'NONE', #8612 ) ;
#1796 = CARTESIAN_POINT ( 'NONE',  ( -25.00000000000002487, -45.00000000000000000, 30.00000000000000000 ) ) ;
#1797 = VECTOR ( 'NONE', #6632, 1000.000000000000000 ) ;
#1798 = CARTESIAN_POINT ( 'NONE',  ( -28.49241082802385350, -34.44859572486944188, -9.874625247442173404 ) ) ;
#1799 = CARTESIAN_POINT ( 'NONE',  ( -39.38303923565386100, -50.70000000000000995, -1.486127417882099788 ) ) ;
#1800 = AXIS2_PLACEMENT_3D ( 'NONE', #8129, #2664, #95 ) ;
#1801 = ORIENTED_EDGE ( 'NONE', *, *, #8649, .F. ) ;
#1802 = MECHANICAL_DESIGN_GEOMETRIC_PRESENTATION_REPRESENTATION (  '', ( #7848 ), #242 ) ;
#1803 = CARTESIAN_POINT ( 'NONE',  ( -20.62524821624488069, -36.20140427513057091, 1.538452329860250378 ) ) ;
#1804 = CYLINDRICAL_SURFACE ( 'NONE', #1506, 2.149999999999985256 ) ;
#1805 = CARTESIAN_POINT ( 'NONE',  ( -40.00000000000002842, 1.224646799147353256E-15, -45.00000000000000000 ) ) ;
#1806 = CARTESIAN_POINT ( 'NONE',  ( -41.99999999999996447, 48.00000000000002842, -23.64999999999999858 ) ) ;
#1807 = CARTESIAN_POINT ( 'NONE',  ( 4.200000000000001954, 0.000000000000000000, 0.000000000000000000 ) ) ;
#1808 = CARTESIAN_POINT ( 'NONE',  ( -4.999999999999998224, -42.92893218813448897, -95.85000000000002274 ) ) ;
#1809 = ORIENTED_EDGE ( 'NONE', *, *, #3323, .T. ) ;
#1810 = CARTESIAN_POINT ( 'NONE',  ( -33.85891924778610473, -41.10000000000000142, 7.573555455601171715 ) ) ;
#1811 = ORIENTED_EDGE ( 'NONE', *, *, #5412, .T. ) ;
#1812 = EDGE_CURVE ( 'NONE', #3910, #2290, #1912, .T. ) ;
#1813 = CARTESIAN_POINT ( 'NONE',  ( 9.184850993605145972E-16, -49.99999999999997158, -98.00000000000000000 ) ) ;
#1814 = CARTESIAN_POINT ( 'NONE',  ( -4.680199288021800186, -46.85220489305395830, -100.0000024770419884 ) ) ;
#1815 = FACE_OUTER_BOUND ( 'NONE', #4053, .T. ) ;
#1816 = DIRECTION ( 'NONE',  ( -0.5150380749100560429, 0.000000000000000000, 0.8571673007021112234 ) ) ;
#1817 = CLOSED_SHELL ( 'NONE', ( #4289, #8553, #3851, #60, #7347, #1105, #364, #5005, #281, #6132, #4960, #6122, #1572, #351, #4484, #214, #5595, #8637, #619, #7965, #666, #1368, #1655, #4170 ) ) ;
#1818 = ADVANCED_FACE ( 'NONE', ( #6047 ), #1375, .F. ) ;
#1819 = LINE ( 'NONE', #518, #4339 ) ;
#1820 = DIRECTION ( 'NONE',  ( 0.000000000000000000, 0.000000000000000000, 1.000000000000000000 ) ) ;
#1821 = DIRECTION ( 'NONE',  ( 0.000000000000000000, -1.000000000000000000, 8.560894001270036306E-16 ) ) ;
#1822 = EDGE_CURVE ( 'NONE', #3764, #5405, #618, .T. ) ;
#1823 = CARTESIAN_POINT ( 'NONE',  ( -20.13408869516454303, -49.05000000000000426, -1.562606840307982692 ) ) ;
#1824 = DIRECTION ( 'NONE',  ( 6.123233995736766036E-17, -1.000000000000000000, 0.000000000000000000 ) ) ;
#1825 = ORIENTED_EDGE ( 'NONE', *, *, #2748, .T. ) ;
#1826 = CARTESIAN_POINT ( 'NONE',  ( -31.34310424141748896, -47.94859572486943478, 8.836108267985801845 ) ) ;
#1827 = CARTESIAN_POINT ( 'NONE',  ( -38.90016716647221529, -32.85000000000000853, -4.534861676072185155 ) ) ;
#1828 = CARTESIAN_POINT ( 'NONE',  ( -26.09387776718931917, -41.60140427513058370, -7.549504333439021941 ) ) ;
#1829 = CARTESIAN_POINT ( 'NONE',  ( -3.061616997868382155E-16, -39.99999999999997158, -96.00000000000000000 ) ) ;
#1830 = CARTESIAN_POINT ( 'NONE',  ( -34.35889894354067309, 9.000000000000001776, 125.0000000000000000 ) ) ;
#1831 = CARTESIAN_POINT ( 'NONE',  ( -34.58449383169706692, -34.14859572486943051, -8.874878320068054549 ) ) ;
#1832 = CARTESIAN_POINT ( 'NONE',  ( -28.43739315969223824, -39.45000000000000995, -9.865911304835512041 ) ) ;
#1833 = CARTESIAN_POINT ( 'NONE',  ( -1.891708078845683039, -40.43301269999998482, -99.59999999890754907 ) ) ;
#1834 = CYLINDRICAL_SURFACE ( 'NONE', #3445, 12.49999999999997691 ) ;
#1835 = CARTESIAN_POINT ( 'NONE',  ( 3.229347689422839895, -41.77065231057713390, -96.34999999890753486 ) ) ;
#1836 = ADVANCED_FACE ( 'NONE', ( #7327, #2622, #667, #5251, #9, #3418, #8694 ), #1200, .T. ) ;
#1837 =( LENGTH_UNIT ( ) NAMED_UNIT ( * ) SI_UNIT ( .MILLI., .METRE. ) );
#1838 = CIRCLE ( 'NONE', #2539, 12.65000000000000036 ) ;
#1839 = ORIENTED_EDGE ( 'NONE', *, *, #2379, .F. ) ;
#1840 = CARTESIAN_POINT ( 'NONE',  ( -33.35889894354067309, -8.999999999999998224, 124.0000000000000000 ) ) ;
#1841 = CARTESIAN_POINT ( 'NONE',  ( -36.75497492228666374, -30.99859572486944259, -6.680053920257780220 ) ) ;
#1842 = CARTESIAN_POINT ( 'NONE',  ( -37.06321265474346660, -50.24999999999998579, 7.063212654743582952 ) ) ;
#1843 = PRODUCT_DEFINITION ( 'UNKNOWN', '', #6919, #7580 ) ;
#1844 = ORIENTED_EDGE ( 'NONE', *, *, #5468, .T. ) ;
#1845 = ORIENTED_EDGE ( 'NONE', *, *, #7701, .T. ) ;
#1846 = CARTESIAN_POINT ( 'NONE',  ( -34.48522952044771017, -38.15140427513058086, -8.925456012876139766 ) ) ;
#1847 = CARTESIAN_POINT ( 'NONE',  ( 4.999999999999998224, -42.92893218813449607, -96.84999999781504698 ) ) ;
#1848 = LINE ( 'NONE', #3787, #7361 ) ;
#1849 = DIRECTION ( 'NONE',  ( -1.000000000000000000, 0.000000000000000000, 0.000000000000000000 ) ) ;
#1850 = CARTESIAN_POINT ( 'NONE',  ( -4.999999999999998224, -42.92893218813448897, -97.44999999999998863 ) ) ;
#1851 = ADVANCED_FACE ( 'NONE', ( #7906, #1872 ), #572, .F. ) ;
#1852 = ORIENTED_EDGE ( 'NONE', *, *, #1071, .F. ) ;
#1853 = CARTESIAN_POINT ( 'NONE',  ( -33.85891924778610473, -44.10000000000000853, 7.573555455601171715 ) ) ;
#1854 = EDGE_CURVE ( 'NONE', #7457, #1434, #7240, .T. ) ;
#1855 = MECHANICAL_DESIGN_GEOMETRIC_PRESENTATION_REPRESENTATION (  '', ( #1718 ), #3962 ) ;
#1856 = EDGE_LOOP ( 'NONE', ( #3697, #6178 ) ) ;
#1857 = CARTESIAN_POINT ( 'NONE',  ( 2.071067811865477282, -49.99999999999996447, -98.75000000000001421 ) ) ;
#1858 = CARTESIAN_POINT ( 'NONE',  ( -3.596541285565526991, -41.51505981109065146, -100.0002518188403116 ) ) ;
#1859 = CARTESIAN_POINT ( 'NONE',  ( -25.99212434019154472, -36.65140427513058086, 7.988596311142242890 ) ) ;
#1860 = AXIS2_PLACEMENT_3D ( 'NONE', #1322, #2662, #5204 ) ;
#1861 = DIRECTION ( 'NONE',  ( -0.000000000000000000, -1.000000000000000000, -0.000000000000000000 ) ) ;
#1862 = VECTOR ( 'NONE', #8209, 999.9999999999998863 ) ;
#1863 = CARTESIAN_POINT ( 'NONE',  ( -22.03669253526174998, -34.35000000000000853, 4.057507815433014642 ) ) ;
#1864 = CARTESIAN_POINT ( 'NONE',  ( 4.999999999999998224, -44.99999999999997158, -96.09999999781504698 ) ) ;
#1865 = CARTESIAN_POINT ( 'NONE',  ( -20.13408869516454303, -46.05000000000000426, -1.562606840307982692 ) ) ;
#1866 = CARTESIAN_POINT ( 'NONE',  ( 0.000000000000000000, -81.00000000000001421, 0.000000000000000000 ) ) ;
#1867 = EDGE_LOOP ( 'NONE', ( #8128, #692, #1960, #753 ) ) ;
#1868 = CARTESIAN_POINT ( 'NONE',  ( -21.18131961722757595, -50.04859572486944330, -1.453139578080854699 ) ) ;
#1869 = CARTESIAN_POINT ( 'NONE',  ( -31.56260684030781505, -34.95000000000000995, 9.865911304835510265 ) ) ;
#1870 = VECTOR ( 'NONE', #6682, 1000.000000000000000 ) ;
#1871 = CARTESIAN_POINT ( 'NONE',  ( -28.54686042191934092, -41.45140427513058512, -8.818680382772479120 ) ) ;
#1872 = FACE_OUTER_BOUND ( 'NONE', #3259, .T. ) ;
#1873 = CARTESIAN_POINT ( 'NONE',  ( 34.99999999999998579, -44.99999999999995737, 11.45643923738957071 ) ) ;
#1874 = CARTESIAN_POINT ( 'NONE',  ( -38.44051085762733777, -39.39859572486943762, 4.360112732550414982 ) ) ;
#1875 = CARTESIAN_POINT ( 'NONE',  ( -38.46456197978948666, -32.40000000000000568, 4.312909747525784709 ) ) ;
#1876 = DIRECTION ( 'NONE',  ( -0.000000000000000000, 1.000000000000000000, -0.000000000000000000 ) ) ;
#1877 = DIRECTION ( 'NONE',  ( 0.000000000000000000, 0.000000000000000000, 1.000000000000000000 ) ) ;
#1878 = CIRCLE ( 'NONE', #881, 11.99999999999983302 ) ;
#1879 = CARTESIAN_POINT ( 'NONE',  ( 4.566987299999998307, -44.99999999999997158, -95.64999999890753202 ) ) ;
#1880 = ORIENTED_EDGE ( 'NONE', *, *, #486, .T. ) ;
#1881 = LINE ( 'NONE', #4566, #597 ) ;
#1882 = CARTESIAN_POINT ( 'NONE',  ( -38.81868038277247734, -51.54859572486944330, 1.453139578080855365 ) ) ;
#1883 = CARTESIAN_POINT ( 'NONE',  ( -34.36011273255026310, -34.10140427513057659, 8.440510857627391061 ) ) ;
#1884 = EDGE_CURVE ( 'NONE', #724, #2594, #7698, .T. ) ;
#1885 = VECTOR ( 'NONE', #2541, 1000.000000000000000 ) ;
#1886 = ORIENTED_EDGE ( 'NONE', *, *, #4542, .F. ) ;
#1887 = VERTEX_POINT ( 'NONE', #1954 ) ;
#1888 = CARTESIAN_POINT ( 'NONE',  ( -20.62524821624488069, -39.20140427513058512, 1.538452329860250378 ) ) ;
#1889 = CARTESIAN_POINT ( 'NONE',  ( 30.00000000000000000, -39.99999999999998579, 12.49999999999996625 ) ) ;
#1890 = LINE ( 'NONE', #7345, #2857 ) ;
#1891 = DIRECTION ( 'NONE',  ( 0.000000000000000000, 0.000000000000000000, 1.000000000000000000 ) ) ;
#1892 = DIRECTION ( 'NONE',  ( -1.000000000000000000, 0.000000000000000000, 0.000000000000000000 ) ) ;
#1893 = AXIS2_PLACEMENT_3D ( 'NONE', #164, #2861, #5536 ) ;
#1894 = ORIENTED_EDGE ( 'NONE', *, *, #4940, .T. ) ;
#1895 = CARTESIAN_POINT ( 'NONE',  ( -36.01040764008574513, -42.00000000000000711, -6.010407640085605685 ) ) ;
#1896 = ORIENTED_EDGE ( 'NONE', *, *, #8180, .T. ) ;
#1897 = DIRECTION ( 'NONE',  ( 1.000000000000000000, 0.000000000000000000, 0.000000000000000000 ) ) ;
#1898 = CARTESIAN_POINT ( 'NONE',  ( -4.999999999999998224, -42.92893218813448897, -97.44999999999998863 ) ) ;
#1899 = CARTESIAN_POINT ( 'NONE',  ( -36.71751442127229836, -48.00000000000000711, -6.717514421272142044 ) ) ;
#1900 = CARTESIAN_POINT ( 'NONE',  ( -4.566987299999998307, -44.99999999999997158, -99.24999999890752633 ) ) ;
#1901 = CARTESIAN_POINT ( 'NONE',  ( -20.00000000000002487, 0.000000000000000000, -40.35000000000000142 ) ) ;
#1902 = CARTESIAN_POINT ( 'NONE',  ( -23.64089511245930098, -29.75140427513057517, -6.280328284105564762 ) ) ;
#1903 = CARTESIAN_POINT ( 'NONE',  ( -4.999999999999998224, -44.99999999999997158, -96.59300000002185982 ) ) ;
#1904 = CARTESIAN_POINT ( 'NONE',  ( -28.60187809025093841, -33.45000000000000995, -8.827394325379140483 ) ) ;
#1905 = DIRECTION ( 'NONE',  ( -0.000000000000000000, -0.000000000000000000, -1.000000000000000000 ) ) ;
#1906 = DIRECTION ( 'NONE',  ( 0.000000000000000000, -0.4999999999999992784, 0.8660254037844389297 ) ) ;
#1907 = VERTEX_POINT ( 'NONE', #5379 ) ;
#1908 = CARTESIAN_POINT ( 'NONE',  ( 2.071067811865477282, -49.99999999999997158, -99.54999999999999716 ) ) ;
#1909 = CARTESIAN_POINT ( 'NONE',  ( -28.51387258211773812, -40.80000000000000426, 9.383039235653802379 ) ) ;
#1910 = CARTESIAN_POINT ( 'NONE',  ( -34.00787565980851213, -44.15140427513058086, -7.988596311142238449 ) ) ;
#1911 = AXIS2_PLACEMENT_3D ( 'NONE', #3063, #5945, #1737 ) ;
#1912 = LINE ( 'NONE', #7949, #2782 ) ;
#1913 = DIRECTION ( 'NONE',  ( 0.000000000000000000, 0.000000000000000000, 1.000000000000000000 ) ) ;
#1914 = CARTESIAN_POINT ( 'NONE',  ( -31.50758917197619979, -38.94859572486943478, 9.874625247442176956 ) ) ;
#1915 = CARTESIAN_POINT ( 'NONE',  ( -34.53486167607238144, -42.15000000000001279, -8.900167166472096270 ) ) ;
#1916 = DIRECTION ( 'NONE',  ( 0.000000000000000000, 0.000000000000000000, 1.000000000000000000 ) ) ;
#1917 = CARTESIAN_POINT ( 'NONE',  ( -7.654042494670954648E-16, -39.99999999999997158, -100.0000000000000000 ) ) ;
#1918 = CARTESIAN_POINT ( 'NONE',  ( 4.566987299999998307, -43.10829192115428299, -98.99999999890751212 ) ) ;
#1919 =( NAMED_UNIT ( * ) SI_UNIT ( $, .STERADIAN. ) SOLID_ANGLE_UNIT ( ) );
#1920 = ORIENTED_EDGE ( 'NONE', *, *, #1055, .F. ) ;
#1921 = CARTESIAN_POINT ( 'NONE',  ( -21.07454398712378918, -32.34859572486942625, 4.485229520447505003 ) ) ;
#1922 = CARTESIAN_POINT ( 'NONE',  ( -20.61696076434619584, -49.20000000000000995, 1.486127417882100676 ) ) ;
#1923 = AXIS2_PLACEMENT_3D ( 'NONE', #7383, #2763, #1336 ) ;
#1924 = EDGE_CURVE ( 'NONE', #6529, #7164, #925, .T. ) ;
#1925 = VERTEX_POINT ( 'NONE', #2532 ) ;
#1926 = AXIS2_PLACEMENT_3D ( 'NONE', #4885, #165, #206 ) ;
#1927 = ORIENTED_EDGE ( 'NONE', *, *, #7948, .F. ) ;
#1928 = CARTESIAN_POINT ( 'NONE',  ( -37.10260095646111012, -49.25140427513058938, 7.023824353025939438 ) ) ;
#1929 = DIRECTION ( 'NONE',  ( -0.000000000000000000, -0.000000000000000000, 1.000000000000000000 ) ) ;
#1930 = CARTESIAN_POINT ( 'NONE',  ( -30.00000000000002487, 0.000000000000000000, -45.00000000000000000 ) ) ;
#1931 = CARTESIAN_POINT ( 'NONE',  ( 5.000000000000000000, -47.07106781186545419, -99.34999999781506119 ) ) ;
#1932 = CARTESIAN_POINT ( 'NONE',  ( 2.000000000000000000, 1.773042676681340968, -1.951563910473907981E-15 ) ) ;
#1933 = CARTESIAN_POINT ( 'NONE',  ( -4.999999999999997335, -47.07106781186546129, -98.15000000000000568 ) ) ;
#1934 = ORIENTED_EDGE ( 'NONE', *, *, #3311, .T. ) ;
#1935 = AXIS2_PLACEMENT_3D ( 'NONE', #8305, #6923, #2178 ) ;
#1936 = CARTESIAN_POINT ( 'NONE',  ( -37.57355545560112375, -41.40000000000000568, 3.858919247786223305 ) ) ;
#1937 = EDGE_CURVE ( 'NONE', #6055, #4623, #6616, .T. ) ;
#1938 = ORIENTED_EDGE ( 'NONE', *, *, #7844, .F. ) ;
#1939 = CARTESIAN_POINT ( 'NONE',  ( 0.000000000000000000, -44.99999999999997158, -95.00000000000000000 ) ) ;
#1940 = CARTESIAN_POINT ( 'NONE',  ( 2.071067811865477282, -49.99999999999996447, -97.04999999781504982 ) ) ;
#1941 = CARTESIAN_POINT ( 'NONE',  ( -21.53543802021056663, -45.90000000000001279, -4.312909747525783821 ) ) ;
#1942 = CARTESIAN_POINT ( 'NONE',  ( 1.891708078845682595, -40.43301269999998482, -98.69999999890752918 ) ) ;
#1943 = CARTESIAN_POINT ( 'NONE',  ( 4.922040131017533682, -43.95328541805098155, -100.0010338072894172 ) ) ;
#1944 = CARTESIAN_POINT ( 'NONE',  ( -26.09387776718931917, -32.60140427513057659, -7.549504333439021941 ) ) ;
#1945 = CARTESIAN_POINT ( 'NONE',  ( 3.535533905932737309, -48.53553390593270933, -97.89300000002185698 ) ) ;
#1946 = CARTESIAN_POINT ( 'NONE',  ( -37.96330746473829976, -35.85000000000000142, -4.057507815433013754 ) ) ;
#1947 = CARTESIAN_POINT ( 'NONE',  ( 29.99999999999997158, 1.102182119232617753E-14, 60.00000000000002842 ) ) ;
#1948 = LINE ( 'NONE', #4503, #6931 ) ;
#1949 = CARTESIAN_POINT ( 'NONE',  ( 42.00000000000000711, 84.00000000000002842, -21.99999999999992184 ) ) ;
#1950 = ORIENTED_EDGE ( 'NONE', *, *, #3451, .T. ) ;
#1951 = FACE_OUTER_BOUND ( 'NONE', #4537, .T. ) ;
#1952 = CARTESIAN_POINT ( 'NONE',  ( -38.90016716647221529, -41.84999999999999432, -4.534861676072185155 ) ) ;
#1953 = CARTESIAN_POINT ( 'NONE',  ( -37.93801861833426159, -49.85140427513058370, -4.107139971057695682 ) ) ;
#1954 = CARTESIAN_POINT ( 'NONE',  ( 44.14999999999999147, 21.99999999999992184, 80.00000000000002842 ) ) ;
#1955 = CARTESIAN_POINT ( 'NONE',  ( 34.83675056951057059, -43.69086006543227541, 11.52652666073311316 ) ) ;
#1956 = CARTESIAN_POINT ( 'NONE',  ( -28.46154767013959486, -32.79859572486943620, 9.374751783755112200 ) ) ;
#1957 = DIRECTION ( 'NONE',  ( -1.000000000000000000, -0.000000000000000000, -0.000000000000000000 ) ) ;
#1958 = DIRECTION ( 'NONE',  ( -0.000000000000000000, 1.000000000000000000, -0.000000000000000000 ) ) ;
#1959 = CARTESIAN_POINT ( 'NONE',  ( -3.229347689422840784, -41.77065231057713390, -99.54999999890752349 ) ) ;
#1960 = ORIENTED_EDGE ( 'NONE', *, *, #4797, .T. ) ;
#1961 = DIRECTION ( 'NONE',  ( -1.000000000000000000, -0.000000000000000000, -0.000000000000000000 ) ) ;
#1962 = CARTESIAN_POINT ( 'NONE',  ( -22.03669253526174998, -46.34999999999998721, 4.057507815433014642 ) ) ;
#1963 = CARTESIAN_POINT ( 'NONE',  ( -26.18828373723858149, -49.59859572486944046, -7.597606577763319713 ) ) ;
#1964 = CARTESIAN_POINT ( 'NONE',  ( -34.31290974752564438, -50.10000000000000853, 8.464561979789547053 ) ) ;
#1965 = ORIENTED_EDGE ( 'NONE', *, *, #7880, .T. ) ;
#1966 = ORIENTED_EDGE ( 'NONE', *, *, #7163, .F. ) ;
#1967 = CARTESIAN_POINT ( 'NONE',  ( -23.31994607974211675, -42.50140427513057517, 6.754974922286503869 ) ) ;
#1968 = DIRECTION ( 'NONE',  ( 0.7061138087190598212, -0.05297714858780431385, -0.7061138087190823587 ) ) ;
#1969 = AXIS2_PLACEMENT_3D ( 'NONE', #6964, #3095, #5117 ) ;
#1970 = CARTESIAN_POINT ( 'NONE',  ( -4.999999999999997335, -47.07106781186546129, -99.64999999781502993 ) ) ;
#1971 = CARTESIAN_POINT ( 'NONE',  ( -3.535533905932736864, -41.46446609406723383, -95.10000000000000853 ) ) ;
#1972 = CARTESIAN_POINT ( 'NONE',  ( -3.535533905932736864, -41.46446609406723383, -99.10000000000000853 ) ) ;
#1973 =( BOUNDED_CURVE ( )  B_SPLINE_CURVE ( 2, ( #4087, #5225, #2726, #7924, #3345, #5936, #2640, #3304, #3389 ),
 .UNSPECIFIED., .F., .T. ) 
 B_SPLINE_CURVE_WITH_KNOTS ( ( 3, 2, 2, 2, 3 ),
 ( 0.7142857142857143016, 0.7321428571428570953, 0.7500000000000000000, 0.7678571428571429047, 0.7857142857142856984 ),
 .UNSPECIFIED. ) 
 CURVE ( )  GEOMETRIC_REPRESENTATION_ITEM ( )  RATIONAL_B_SPLINE_CURVE ( ( 1.000000000000000000, 0.9238795325112867385, 1.000000000000000000, 0.9238795325112867385, 1.000000000000000000, 0.9238795325112867385, 1.000000000000000000, 0.9238795325112867385, 1.000000000000000000 ) ) 
 REPRESENTATION_ITEM ( '' )  );
#1974 = EDGE_CURVE ( 'NONE', #5482, #1354, #5414, .T. ) ;
#1975 = VERTEX_POINT ( 'NONE', #7631 ) ;
#1976 = CARTESIAN_POINT ( 'NONE',  ( -21.60464910494133406, -46.20000000000000284, 1.329692952841886155 ) ) ;
#1977 = DIRECTION ( 'NONE',  ( -1.000000000000000000, 0.000000000000000000, 0.000000000000000000 ) ) ;
#1978 = AXIS2_PLACEMENT_3D ( 'NONE', #4643, #7423, #7331 ) ;
#1979 = ORIENTED_EDGE ( 'NONE', *, *, #2086, .F. ) ;
#1980 = CARTESIAN_POINT ( 'NONE',  ( 4.566987300000000083, -46.89170807884564596, -99.09999999890752065 ) ) ;
#1981 = CARTESIAN_POINT ( 'NONE',  ( 4.999999999999998224, -42.92893218813448897, -96.04999999781504982 ) ) ;
#1982 = CIRCLE ( 'NONE', #5347, 1.000000000000000888 ) ;
#1983 = CARTESIAN_POINT ( 'NONE',  ( -20.13408869516453947, -46.05000000000001137, -1.562606840307983136 ) ) ;
#1984 = CARTESIAN_POINT ( 'NONE',  ( -4.566987299999998307, -43.10829192115428299, -98.49999999890752633 ) ) ;
#1985 = LINE ( 'NONE', #651, #1414 ) ;
#1986 = CARTESIAN_POINT ( 'NONE',  ( -38.83610826798580717, -31.55140427513057588, 1.343104241417631073 ) ) ;
#1987 =( GEOMETRIC_REPRESENTATION_CONTEXT ( 3 ) GLOBAL_UNCERTAINTY_ASSIGNED_CONTEXT ( ( #3854 ) ) GLOBAL_UNIT_ASSIGNED_CONTEXT ( ( #8044, #1334, #536 ) ) REPRESENTATION_CONTEXT ( 'NONE', 'WORKASPACE' ) );
#1988 = EDGE_CURVE ( 'NONE', #4697, #4311, #890, .T. ) ;
#1989 = CARTESIAN_POINT ( 'NONE',  ( -3.061616997868382155E-16, -39.99999999999997158, -95.19300000002185413 ) ) ;
#1990 = CARTESIAN_POINT ( 'NONE',  ( -31.39812190974910422, -34.95000000000000995, 8.827394325379140483 ) ) ;
#1991 = FACE_OUTER_BOUND ( 'NONE', #3804, .T. ) ;
#1992 = CARTESIAN_POINT ( 'NONE',  ( -25.46513832392766119, -49.64999999999999858, 8.900167166472096270 ) ) ;
#1993 = DIRECTION ( 'NONE',  ( 0.000000000000000000, 1.000000000000000000, 0.000000000000000000 ) ) ;
#1994 = ORIENTED_EDGE ( 'NONE', *, *, #7332, .T. ) ;
#1995 = LINE ( 'NONE', #6136, #7420 ) ;
#1996 = CARTESIAN_POINT ( 'NONE',  ( -23.28248557872775137, -43.50000000000001421, 6.717514421272141156 ) ) ;
#1997 = CARTESIAN_POINT ( 'NONE',  ( -25.94249218456686279, -31.65000000000000568, 7.963307464738195840 ) ) ;
#1998 = CARTESIAN_POINT ( 'NONE',  ( 2.071067811865477282, -49.99999999999996447, -97.94300000002185413 ) ) ;
#1999 = DIRECTION ( 'NONE',  ( -0.000000000000000000, -0.000000000000000000, -1.000000000000000000 ) ) ;
#2000 = PLANE ( 'NONE',  #2928 ) ;
#2001 = CARTESIAN_POINT ( 'NONE',  ( -34.26570676250101855, -33.09859572486943335, 8.488613101951703044 ) ) ;
#2002 = CARTESIAN_POINT ( 'NONE',  ( 0.000000000000000000, -44.99999999999997158, -95.00000000000000000 ) ) ;
#2003 = PLANE ( 'NONE',  #4144 ) ;
#2004 = CARTESIAN_POINT ( 'NONE',  ( -4.566987299999997418, -46.89170807884566727, -95.99999999890752633 ) ) ;
#2006 = CIRCLE ( 'NONE', #579, 1.649999999999998579 ) ;
#2005 =( NAMED_UNIT ( * ) PLANE_ANGLE_UNIT ( ) SI_UNIT ( $, .RADIAN. ) );
#2007 = ORIENTED_EDGE ( 'NONE', *, *, #3451, .F. ) ;
#2008 = DIRECTION ( 'NONE',  ( -0.000000000000000000, -0.000000000000000000, 1.000000000000000000 ) ) ;
#2009 = CARTESIAN_POINT ( 'NONE',  ( -31.32969295284206979, -45.30000000000000426, -8.395350895058669494 ) ) ;
#2010 = CARTESIAN_POINT ( 'NONE',  ( -34.58449383169706692, -40.14859572486943762, -8.874878320068054549 ) ) ;
#2011 = CARTESIAN_POINT ( 'NONE',  ( -31.61762450863942320, -39.95140427513058512, 9.857197362228843573 ) ) ;
#2012 = VERTEX_POINT ( 'NONE', #6797 ) ;
#2013 = VECTOR ( 'NONE', #92, 1000.000000000000000 ) ;
#2014 = EDGE_LOOP ( 'NONE', ( #6914, #542 ) ) ;
#2015 = CARTESIAN_POINT ( 'NONE',  ( -39.87462524744216807, -43.55140427513057944, 1.507589171976367215 ) ) ;
#2016 = PRESENTATION_LAYER_ASSIGNMENT (  '', '', ( #39 ) ) ;
#2017 = CARTESIAN_POINT ( 'NONE',  ( 4.999999999999998224, -44.99999999999997158, -95.40000000000000568 ) ) ;
#2018 = DIRECTION ( 'NONE',  ( 1.000000000000000000, -0.000000000000000000, -0.000000000000000000 ) ) ;
#2019 = CARTESIAN_POINT ( 'NONE',  ( -4.999999999999997335, -47.07106781186546129, -100.4499999978150413 ) ) ;
#2020 = DIRECTION ( 'NONE',  ( 1.000000000000000000, 0.000000000000000000, 0.000000000000000000 ) ) ;
#2021 = DIRECTION ( 'NONE',  ( -0.000000000000000000, 0.000000000000000000, 1.000000000000000000 ) ) ;
#2022 = EDGE_LOOP ( 'NONE', ( #6847, #3430 ) ) ;
#2023 = CARTESIAN_POINT ( 'NONE',  ( -38.81868038277247734, -33.54859572486944330, 1.453139578080855365 ) ) ;
#2024 = CARTESIAN_POINT ( 'NONE',  ( -23.28248557872775137, -31.50000000000000711, 6.717514421272141156 ) ) ;
#2025 = CIRCLE ( 'NONE', #4694, 3.500000000000000000 ) ;
#2026 = ADVANCED_FACE ( 'NONE', ( #6094 ), #1595, .F. ) ;
#2027 = ORIENTED_EDGE ( 'NONE', *, *, #7899, .T. ) ;
#2028 = CARTESIAN_POINT ( 'NONE',  ( -4.566987299999998307, -43.10829192115428299, -96.29999999890752349 ) ) ;
#2029 = CARTESIAN_POINT ( 'NONE',  ( -4.999999999999998224, -44.99999999999997158, -97.29999999781504982 ) ) ;
#2030 = CARTESIAN_POINT ( 'NONE',  ( -25.68709025247441602, -39.60000000000000853, -8.464561979789547053 ) ) ;
#2031 = CARTESIAN_POINT ( 'NONE',  ( -4.566987299999998307, -44.99999999999997158, -98.44999999890752918 ) ) ;
#2032 = SURFACE_STYLE_USAGE ( .BOTH. , #744 ) ;
#2033 = CARTESIAN_POINT ( 'NONE',  ( -31.27736804086391942, -32.30140427513056522, -8.403638346957361449 ) ) ;
#2034 = CIRCLE ( 'NONE', #1893, 12.00000000000004263 ) ;
#2035 = CARTESIAN_POINT ( 'NONE',  ( -3.535533905932735532, -48.53553390593270933, -95.69300000002185413 ) ) ;
#2036 = CARTESIAN_POINT ( 'NONE',  ( -22.03669253526174998, -49.35000000000000853, 4.057507815433014642 ) ) ;
#2037 = CARTESIAN_POINT ( 'NONE',  ( 39.85000000000002274, 21.99999999999992184, 80.00000000000002842 ) ) ;
#2038 = DIRECTION ( 'NONE',  ( 1.000000000000000000, 0.000000000000000000, 0.000000000000000000 ) ) ;
#2039 = CONTEXT_DEPENDENT_SHAPE_REPRESENTATION ( #8024, #353 ) ;
#2040 = ORIENTED_EDGE ( 'NONE', *, *, #2379, .T. ) ;
#2041 = LINE ( 'NONE', #615, #2787 ) ;
#2042 = CARTESIAN_POINT ( 'NONE',  ( -39.38303923565386100, -44.70000000000000284, -1.486127417882099788 ) ) ;
#2043 = CARTESIAN_POINT ( 'NONE',  ( -36.35910488754074521, -46.25140427513058228, 6.280328284105565650 ) ) ;
#2044 = EDGE_CURVE ( 'NONE', #1415, #5592, #3469, .T. ) ;
#2045 = CARTESIAN_POINT ( 'NONE',  ( 42.00000000000000711, 48.00000000000002842, -21.99999999999992184 ) ) ;
#2046 = CARTESIAN_POINT ( 'NONE',  ( -25.00000000000002487, -45.00000000000000000, -30.00100000000000122 ) ) ;
#2047 = CARTESIAN_POINT ( 'NONE',  ( -23.24502507771338600, -47.49859572486944614, 6.680053920257780220 ) ) ;
#2048 = CARTESIAN_POINT ( 'NONE',  ( -10.00000000000000000, 0.000000000000000000, 1.622657008870243228E-16 ) ) ;
#2049 = CARTESIAN_POINT ( 'NONE',  ( -25.46513832392766119, -31.65000000000000568, 8.900167166472096270 ) ) ;
#2050 = CARTESIAN_POINT ( 'NONE',  ( 1.891708078845685481, -49.56698729999997255, -96.59999999890754907 ) ) ;
#2051 = SURFACE_STYLE_FILL_AREA ( #5299 ) ;
#2052 = ORIENTED_EDGE ( 'NONE', *, *, #723, .T. ) ;
#2053 = DIRECTION ( 'NONE',  ( 1.000000000000000000, 0.000000000000000000, 0.000000000000000000 ) ) ;
#2054 = VECTOR ( 'NONE', #4822, 1000.000000000000000 ) ;
#2055 = CARTESIAN_POINT ( 'NONE',  ( -34.05750781543318340, -48.15000000000001279, -7.963307464738195840 ) ) ;
#2056 = CARTESIAN_POINT ( 'NONE',  ( -36.75497492228666374, -36.99859572486943193, -6.680053920257780220 ) ) ;
#2057 = CARTESIAN_POINT ( 'NONE',  ( -20.62524821624488069, -45.20140427513059223, 1.538452329860250378 ) ) ;
#2058 = ORIENTED_EDGE ( 'NONE', *, *, #2254, .T. ) ;
#2059 = VERTEX_POINT ( 'NONE', #2931 ) ;
#2060 = CARTESIAN_POINT ( 'NONE',  ( -25.63988726744978663, -41.60140427513058370, -8.440510857627391061 ) ) ;
#2061 = FACE_OUTER_BOUND ( 'NONE', #7222, .T. ) ;
#2062 = CIRCLE ( 'NONE', #6979, 1.649999999999998579 ) ;
#2063 = DIRECTION ( 'NONE',  ( -1.000000000000000000, -0.000000000000000000, -0.000000000000000000 ) ) ;
#2064 = CARTESIAN_POINT ( 'NONE',  ( -3.535533905932735532, -48.53553390593270933, -98.79999999781504982 ) ) ;
#2065 = DIRECTION ( 'NONE',  ( -1.000000000000000000, -0.000000000000000000, -0.000000000000000000 ) ) ;
#2066 = CARTESIAN_POINT ( 'NONE',  ( 4.999999999999998224, -44.99999999999997158, -95.00000000000000000 ) ) ;
#2067 = ORIENTED_EDGE ( 'NONE', *, *, #746, .F. ) ;
#2068 = CIRCLE ( 'NONE', #6142, 2.099999999999997868 ) ;
#2069 = CARTESIAN_POINT ( 'NONE',  ( -22.01140368885771892, -35.34859572486944046, 4.007875659808335378 ) ) ;
#2070 = CARTESIAN_POINT ( 'NONE',  ( -28.51387258211773812, -31.80000000000000782, 9.383039235653802379 ) ) ;
#2071 = ORIENTED_EDGE ( 'NONE', *, *, #4679, .T. ) ;
#2072 = VERTEX_POINT ( 'NONE', #5467 ) ;
#2073 = CARTESIAN_POINT ( 'NONE',  ( 3.229347689422841228, -48.22934768942280925, -96.74999999890751212 ) ) ;
#2074 = CARTESIAN_POINT ( 'NONE',  ( 3.535533905932737309, -48.53553390593270933, -97.79999999781504982 ) ) ;
#2075 = CARTESIAN_POINT ( 'NONE',  ( -38.46456197978948666, -41.40000000000000568, 4.312909747525784709 ) ) ;
#2076 = CARTESIAN_POINT ( 'NONE',  ( 1.891708078845682595, -40.43301269999998482, -99.49999999890754054 ) ) ;
#2077 =( NAMED_UNIT ( * ) PLANE_ANGLE_UNIT ( ) SI_UNIT ( $, .RADIAN. ) );
#2078 = CARTESIAN_POINT ( 'NONE',  ( -21.61293655684001536, -48.20140427513058512, 1.382017864820032971 ) ) ;
#2079 = TOROIDAL_SURFACE ( 'NONE', #6998, 3.299999999999999822, 0.2000000000000000111 ) ;
#2080 = EDGE_CURVE ( 'NONE', #8009, #3178, #1199, .T. ) ;
#2081 = VECTOR ( 'NONE', #226, 1000.000000000000000 ) ;
#2082 = CARTESIAN_POINT ( 'NONE',  ( 2.071067811865477282, -49.99999999999996447, -95.54300000002184845 ) ) ;
#2083 = CARTESIAN_POINT ( 'NONE',  ( -26.14108075221394856, -42.60000000000000853, -7.573555455601170827 ) ) ;
#2084 = CARTESIAN_POINT ( 'NONE',  ( 27.76939715822961219, -49.48683715626706459, 12.30316928347422412 ) ) ;
#2085 = DIRECTION ( 'NONE',  ( -1.000000000000000000, -0.000000000000000000, 0.000000000000000000 ) ) ;
#2086 = EDGE_CURVE ( 'NONE', #6099, #5583, #7543, .T. ) ;
#2087 = APPLICATION_PROTOCOL_DEFINITION ( 'draft international standard', 'automotive_design', 1998, #3360 ) ;
#2088 = ORIENTED_EDGE ( 'NONE', *, *, #4214, .T. ) ;
#2089 = DIRECTION ( 'NONE',  ( -0.000000000000000000, 1.000000000000000000, -0.000000000000000000 ) ) ;
#2090 = AXIS2_PLACEMENT_3D ( 'NONE', #8601, #2568, #6479 ) ;
#2091 = CARTESIAN_POINT ( 'NONE',  ( -37.06321265474346660, -47.25000000000000711, 7.063212654743582952 ) ) ;
#2092 = CARTESIAN_POINT ( 'NONE',  ( -38.39535089505872634, -32.70000000000000995, -1.329692952841885267 ) ) ;
#2093 = CARTESIAN_POINT ( 'NONE',  ( -25.00000000000001776, -44.67046583110986546, 11.45643923738959025 ) ) ;
#2094 = EDGE_CURVE ( 'NONE', #4829, #2602, #7056, .T. ) ;
#2095 = DIRECTION ( 'NONE',  ( 0.000000000000000000, 0.000000000000000000, -1.000000000000000000 ) ) ;
#2096 = CARTESIAN_POINT ( 'NONE',  ( -20.60867331244750034, -47.19859572486943478, 1.433802505903951419 ) ) ;
#2097 = DIRECTION ( 'NONE',  ( 0.000000000000000000, 0.000000000000000000, -1.000000000000000000 ) ) ;
#2098 = CARTESIAN_POINT ( 'NONE',  ( -20.13408869516454303, -31.05000000000000426, -1.562606840307982692 ) ) ;
#2099 = FILL_AREA_STYLE_COLOUR ( '', #5504 ) ;
#2100 = EDGE_LOOP ( 'NONE', ( #717, #1515, #1460, #4122, #4292 ) ) ;
#2101 = DIRECTION ( 'NONE',  ( 0.000000000000000000, 0.000000000000000000, 1.000000000000000000 ) ) ;
#2102 = CARTESIAN_POINT ( 'NONE',  ( -22.42644454439892598, -48.90000000000000568, -3.858919247786222861 ) ) ;
#2103 = EDGE_CURVE ( 'NONE', #8149, #1617, #1365, .T. ) ;
#2104 = CARTESIAN_POINT ( 'NONE',  ( -31.53845232986046554, -37.29859572486943620, -9.374751783755117529 ) ) ;
#2105 = CARTESIAN_POINT ( 'NONE',  ( -37.10260095646111012, -40.25140427513058228, 7.023824353025939438 ) ) ;
#2106 = CLOSED_SHELL ( 'NONE', ( #6255, #4257, #3642, #3016 ) ) ;
#2107 = EDGE_LOOP ( 'NONE', ( #2052, #1513, #1221, #4024 ) ) ;
#2108 = ORIENTED_EDGE ( 'NONE', *, *, #5306, .F. ) ;
#2109 = CARTESIAN_POINT ( 'NONE',  ( -39.37475178375516549, -43.70140427513058512, -1.538452329860249712 ) ) ;
#2110 = FILL_AREA_STYLE_COLOUR ( '', #8071 ) ;
#2111 = CARTESIAN_POINT ( 'NONE',  ( -26.64110105645932336, -7.999999999999996447, 125.0000000000000000 ) ) ;
#2112 = CARTESIAN_POINT ( 'NONE',  ( 2.071067811865474173, -39.99999999999997158, -99.94999999781505551 ) ) ;
#2113 = DIRECTION ( 'NONE',  ( -1.000000000000000000, -0.000000000000000000, -0.000000000000000000 ) ) ;
#2114 = DIRECTION ( 'NONE',  ( 0.000000000000000000, -0.000000000000000000, -1.000000000000000000 ) ) ;
#2115 = ORIENTED_EDGE ( 'NONE', *, *, #5667, .F. ) ;
#2116 = CARTESIAN_POINT ( 'NONE',  ( -37.54950433343896776, -33.39859572486943762, 3.906122232810848249 ) ) ;
#2117 = CARTESIAN_POINT ( 'NONE',  ( -22.93678734525658314, -36.75000000000000711, -7.063212654743582952 ) ) ;
#2118 = ORIENTED_EDGE ( 'NONE', *, *, #4689, .F. ) ;
#2119 = VECTOR ( 'NONE', #5796, 1000.000000000000000 ) ;
#2120 = FILL_AREA_STYLE_COLOUR ( '', #3766 ) ;
#2121 = CARTESIAN_POINT ( 'NONE',  ( -3.229347689422840784, -41.77065231057713390, -96.34999999890752065 ) ) ;
#2122 = CARTESIAN_POINT ( 'NONE',  ( -3.535533905932735532, -48.53553390593270933, -96.39999999781505835 ) ) ;
#2123 = CARTESIAN_POINT ( 'NONE',  ( -38.46456197978948666, -50.40000000000000568, 4.312909747525784709 ) ) ;
#2124 = CARTESIAN_POINT ( 'NONE',  ( 3.229347689422839895, -41.77065231057713390, -97.94999999890751496 ) ) ;
#2125 =( REPRESENTATION_RELATIONSHIP ('NONE','NONE', #2265, #7097 ) REPRESENTATION_RELATIONSHIP_WITH_TRANSFORMATION ( #2353 )SHAPE_REPRESENTATION_RELATIONSHIP( ) );
#2126 = EDGE_CURVE ( 'NONE', #94, #4958, #6129, .T. ) ;
#2127 = CARTESIAN_POINT ( 'NONE',  ( 34.00000000000000000, 0.000000000000000000, 1.610000000000000098 ) ) ;
#2128 = CARTESIAN_POINT ( 'NONE',  ( -24.02705286092866643, -39.50140427513058228, 6.047868141099968398 ) ) ;
#2129 = CIRCLE ( 'NONE', #2684, 2.149999999999985256 ) ;
#2130 = CARTESIAN_POINT ( 'NONE',  ( 4.999999999999998224, -42.92893218813448897, -98.54300000002183424 ) ) ;
#2131 = CARTESIAN_POINT ( 'NONE',  ( -28.60187809025093841, -42.45000000000000284, -8.827394325379140483 ) ) ;
#2132 = PLANE ( 'NONE',  #1160 ) ;
#2133 = APPLICATION_PROTOCOL_DEFINITION ( 'draft international standard', 'automotive_design', 1998, #8587 ) ;
#2134 = VECTOR ( 'NONE', #1059, 1000.000000000000000 ) ;
#2135 = ORIENTED_EDGE ( 'NONE', *, *, #4306, .T. ) ;
#2136 = FACE_OUTER_BOUND ( 'NONE', #2557, .T. ) ;
#2137 = CARTESIAN_POINT ( 'NONE',  ( -38.46456197978948666, -50.40000000000000568, 4.312909747525784709 ) ) ;
#2138 = CARTESIAN_POINT ( 'NONE',  ( -28.60187809025093841, -33.45000000000000995, -8.827394325379140483 ) ) ;
#2139 = DIRECTION ( 'NONE',  ( -0.000000000000000000, 1.000000000000000000, -0.000000000000000000 ) ) ;
#2140 = COLOUR_RGB ( '', 0.72549020, 0.75294118, 0.79215686) ;
#2141 = FACE_BOUND ( 'NONE', #3876, .T. ) ;
#2142 = CARTESIAN_POINT ( 'NONE',  ( -34.58449383169706692, -49.14859572486945183, -8.874878320068054549 ) ) ;
#2143 = DIRECTION ( 'NONE',  ( 0.000000000000000000, 0.000000000000000000, 1.000000000000000000 ) ) ;
#2144 = CARTESIAN_POINT ( 'NONE',  ( 2.000000000000000000, 1.329782007511004505, -0.7677500000000018199 ) ) ;
#2145 = ORIENTED_EDGE ( 'NONE', *, *, #7045, .F. ) ;
#2146 = EDGE_LOOP ( 'NONE', ( #409, #4929, #6328, #1397 ) ) ;
#2147 = CARTESIAN_POINT ( 'NONE',  ( -23.68028341417693738, -48.75000000000001421, -6.319716585823198507 ) ) ;
#2148 = CARTESIAN_POINT ( 'NONE',  ( -28.46154767013959486, -38.79859572486943620, 9.374751783755112200 ) ) ;
#2149 = CARTESIAN_POINT ( 'NONE',  ( -39.87462524744216807, -43.55140427513057944, 1.507589171976367215 ) ) ;
#2150 = VERTEX_POINT ( 'NONE', #3923 ) ;
#2151 = CARTESIAN_POINT ( 'NONE',  ( -1.891708078845683705, -49.56698729999997255, -96.69999999890754339 ) ) ;
#2152 = VECTOR ( 'NONE', #1179, 1000.000000000000000 ) ;
#2153 = LINE ( 'NONE', #4839, #8074 ) ;
#2154 = VECTOR ( 'NONE', #1019, 1000.000000000000000 ) ;
#2155 = DIRECTION ( 'NONE',  ( 1.000000000000000000, 0.000000000000000000, -0.000000000000000000 ) ) ;
#2156 = CARTESIAN_POINT ( 'NONE',  ( -4.566987299999998307, -43.10829192115428299, -96.29999999890752349 ) ) ;
#2157 = DIRECTION ( 'NONE',  ( 0.000000000000000000, 0.000000000000000000, 1.000000000000000000 ) ) ;
#2158 = CARTESIAN_POINT ( 'NONE',  ( -26.64110105645932336, -8.999999999999998224, 124.0000000000000000 ) ) ;
#2159 = ORIENTED_EDGE ( 'NONE', *, *, #8544, .F. ) ;
#2160 = CARTESIAN_POINT ( 'NONE',  ( -28.61798213517984024, -35.79859572486943620, 8.387063443159973986 ) ) ;
#2161 = CARTESIAN_POINT ( 'NONE',  ( -31.56260684030781505, -34.95000000000000995, 9.865911304835510265 ) ) ;
#2162 = CIRCLE ( 'NONE', #4410, 10.00000000000000178 ) ;
#2163 = MECHANICAL_DESIGN_GEOMETRIC_PRESENTATION_REPRESENTATION (  '', ( #3433 ), #6648 ) ;
#2164 = ORIENTED_EDGE ( 'NONE', *, *, #1723, .T. ) ;
#2165 = CARTESIAN_POINT ( 'NONE',  ( -38.46456197978948666, -47.40000000000001279, 4.312909747525784709 ) ) ;
#2166 = CARTESIAN_POINT ( 'NONE',  ( 3.229347689422841228, -48.22934768942280925, -98.34999999890752065 ) ) ;
#2167 = CARTESIAN_POINT ( 'NONE',  ( 9.184850993605145972E-16, -49.99999999999997158, -98.69999999781505551 ) ) ;
#2168 = FACE_OUTER_BOUND ( 'NONE', #3180, .T. ) ;
#2169 = CARTESIAN_POINT ( 'NONE',  ( -4.566987299999997418, -46.89170807884566727, -97.59999999890756328 ) ) ;
#2170 = CARTESIAN_POINT ( 'NONE',  ( -23.64089511245930098, -41.75140427513057517, -6.280328284105564762 ) ) ;
#2171 = CARTESIAN_POINT ( 'NONE',  ( -2.071067811865475505, -49.99999999999996447, -95.64999999999999147 ) ) ;
#2172 = FACE_OUTER_BOUND ( 'NONE', #387, .T. ) ;
#2173 = CARTESIAN_POINT ( 'NONE',  ( -25.94249218456686279, -40.65000000000000568, 7.963307464738194952 ) ) ;
#2174 = DIRECTION ( 'NONE',  ( 0.000000000000000000, 0.5150380749100563760, 0.8571673007021110013 ) ) ;
#2175 = VECTOR ( 'NONE', #6200, 1000.000000000000000 ) ;
#2176 = SHAPE_DEFINITION_REPRESENTATION ( #5009, #3450 ) ;
#2177 = VERTEX_POINT ( 'NONE', #4421 ) ;
#2178 = DIRECTION ( 'NONE',  ( -1.000000000000000000, 0.000000000000000000, 0.000000000000000000 ) ) ;
#2179 = CARTESIAN_POINT ( 'NONE',  ( 0.000000000000000000, 0.000000000000000000, 0.000000000000000000 ) ) ;
#2180 = CARTESIAN_POINT ( 'NONE',  ( -36.31971658582311591, -38.25000000000001421, 6.319716585823199395 ) ) ;
#2181 = DIRECTION ( 'NONE',  ( 1.000000000000000000, 0.000000000000000000, 0.000000000000000000 ) ) ;
#2182 = DIRECTION ( 'NONE',  ( -1.000000000000000000, 0.000000000000000000, 0.000000000000000000 ) ) ;
#2183 = CARTESIAN_POINT ( 'NONE',  ( -38.44051085762733777, -51.39859572486944472, 4.360112732550414982 ) ) ;
#2184 = DIRECTION ( 'NONE',  ( 0.000000000000000000, 0.000000000000000000, 1.000000000000000000 ) ) ;
#2185 = CARTESIAN_POINT ( 'NONE',  ( -28.43739315969223824, -30.44999999999999574, -9.865911304835512041 ) ) ;
#2186 =( NAMED_UNIT ( * ) SI_UNIT ( $, .STERADIAN. ) SOLID_ANGLE_UNIT ( ) );
#2187 = ORIENTED_EDGE ( 'NONE', *, *, #4214, .F. ) ;
#2188 = DIRECTION ( 'NONE',  ( 0.000000000000000000, 0.000000000000000000, 1.000000000000000000 ) ) ;
#2189 = ORIENTED_EDGE ( 'NONE', *, *, #504, .F. ) ;
#2190 = CARTESIAN_POINT ( 'NONE',  ( -23.71967171589458445, -40.74859572486943904, -6.359104887540838469 ) ) ;
#2191 = CARTESIAN_POINT ( 'NONE',  ( -34.58449383169706692, -37.14859572486943762, -8.874878320068054549 ) ) ;
#2192 = CARTESIAN_POINT ( 'NONE',  ( -35.97294713907137975, -32.00140427513057517, -6.047868141099968398 ) ) ;
#2193 = ADVANCED_FACE ( 'NONE', ( #5078 ), #6441, .T. ) ;
#2194 = VERTEX_POINT ( 'NONE', #355 ) ;
#2195 = CARTESIAN_POINT ( 'NONE',  ( 8.389419568037416259E-16, -49.56698729999997255, -97.44999999890751496 ) ) ;
#2196 = CARTESIAN_POINT ( 'NONE',  ( -30.00000000000002842, 0.000000000000000000, -41.34999999999999432 ) ) ;
#2197 = DIRECTION ( 'NONE',  ( 0.000000000000000000, 0.000000000000000000, -1.000000000000000000 ) ) ;
#2198 = CARTESIAN_POINT ( 'NONE',  ( -4.566987299999998307, -43.10829192115428299, -98.69999999890752918 ) ) ;
#2199 = CARTESIAN_POINT ( 'NONE',  ( -25.00000000000002487, -45.00000000000000000, 11.45643923738959025 ) ) ;
#2200 = VECTOR ( 'NONE', #1999, 1000.000000000000000 ) ;
#2201 = CARTESIAN_POINT ( 'NONE',  ( 2.000000000000000000, 1.329782007511006503, 0.7677499999999991553 ) ) ;
#2202 = VERTEX_POINT ( 'NONE', #1065 ) ;
#2203 = EDGE_CURVE ( 'NONE', #858, #2422, #3629, .T. ) ;
#2204 = CARTESIAN_POINT ( 'NONE',  ( -26.14108075221394856, -48.60000000000000142, -7.573555455601170827 ) ) ;
#2205 = CARTESIAN_POINT ( 'NONE',  ( -25.46513832392765408, -34.64999999999998437, 8.900167166472096270 ) ) ;
#2206 = ORIENTED_EDGE ( 'NONE', *, *, #2771, .T. ) ;
#2207 = CARTESIAN_POINT ( 'NONE',  ( -20.61696076434619584, -49.20000000000000995, 1.486127417882100676 ) ) ;
#2208 = LINE ( 'NONE', #1531, #8280 ) ;
#2209 = CARTESIAN_POINT ( 'NONE',  ( -2.796473189345805913E-16, -40.43301269999997061, -100.4499999989075292 ) ) ;
#2210 = CARTESIAN_POINT ( 'NONE',  ( 0.9662756667218486140, -39.99999999999997158, -100.7233279560109622 ) ) ;
#2211 = EDGE_CURVE ( 'NONE', #2194, #5592, #8593, .T. ) ;
#2212 = CARTESIAN_POINT ( 'NONE',  ( -30.00000000000000000, -49.99999999999997158, -12.49999999999997335 ) ) ;
#2213 = CARTESIAN_POINT ( 'NONE',  ( -4.566987299999998307, -44.99999999999997158, -97.64999999890753202 ) ) ;
#2214 = CARTESIAN_POINT ( 'NONE',  ( -36.35910488754074521, -40.25140427513058228, 6.280328284105565650 ) ) ;
#2215 =( BOUNDED_CURVE ( )  B_SPLINE_CURVE ( 2, ( #7105, #8436, #5781, #5077, #3884, #5911, #8476 ),
 .UNSPECIFIED., .F., .T. ) 
 B_SPLINE_CURVE_WITH_KNOTS ( ( 3, 2, 2, 3 ),
 ( 0.7142857142857143016, 0.7321428571428570953, 0.7500000000000000000, 0.7678571432794624174 ),
 .UNSPECIFIED. ) 
 CURVE ( )  GEOMETRIC_REPRESENTATION_ITEM ( )  RATIONAL_B_SPLINE_CURVE ( ( 1.000000000000000000, 0.9238795325112867385, 1.000000000000000000, 0.9238795325112867385, 1.000000000000000000, 0.9238795325112867385, 1.000000000000000000 ) ) 
 REPRESENTATION_ITEM ( '' )  );
#2216 = ADVANCED_FACE ( 'NONE', ( #6311 ), #4586, .F. ) ;
#2217 = CARTESIAN_POINT ( 'NONE',  ( -4.999999999999998224, -42.92893218813448897, -95.85000000000002274 ) ) ;
#2218 = PRODUCT_DEFINITION_CONTEXT ( 'detailed design', #7404, 'design' ) ;
#2219 = CARTESIAN_POINT ( 'NONE',  ( -1.891708078845683483, -49.56698729999997255, -96.69999999890755760 ) ) ;
#2220 = CARTESIAN_POINT ( 'NONE',  ( -21.17260567462091103, -43.04999999999999716, -1.398121909749241887 ) ) ;
#2221 = EDGE_CURVE ( 'NONE', #5592, #1415, #7114, .T. ) ;
#2222 = CARTESIAN_POINT ( 'NONE',  ( -4.999999999999998224, -42.92893218813449607, -95.74999999781503845 ) ) ;
#2223 = CONTEXT_DEPENDENT_SHAPE_REPRESENTATION ( #8312, #4375 ) ;
#2224 = CARTESIAN_POINT ( 'NONE',  ( -3.535533905932736864, -41.46446609406723383, -100.5999999978150470 ) ) ;
#2225 = CARTESIAN_POINT ( 'NONE',  ( -22.42644454439892598, -42.90000000000000568, -3.858919247786222861 ) ) ;
#2226 = PRODUCT_DEFINITION ( 'UNKNOWN', '', #1570, #3538 ) ;
#2227 = CARTESIAN_POINT ( 'NONE',  ( 25.25924940455542611, -43.37701935357445393, 11.56693546130993155 ) ) ;
#2228 = AXIS2_PLACEMENT_3D ( 'NONE', #7409, #4591, #5955 ) ;
#2229 = CARTESIAN_POINT ( 'NONE',  ( 42.00000000000000711, 21.99999999999992184, 80.00000000000002842 ) ) ;
#2230 = CARTESIAN_POINT ( 'NONE',  ( -38.90016716647221529, -32.85000000000000853, -4.534861676072185155 ) ) ;
#2231 = DIRECTION ( 'NONE',  ( -0.7071067811865587860, 0.000000000000000000, -0.7071067811865362485 ) ) ;
#2232 = CARTESIAN_POINT ( 'NONE',  ( -39.38303923565386100, -35.70000000000000995, -1.486127417882099788 ) ) ;
#2233 = ORIENTED_EDGE ( 'NONE', *, *, #6027, .F. ) ;
#2234 = DIRECTION ( 'NONE',  ( 0.000000000000000000, 0.000000000000000000, 1.000000000000000000 ) ) ;
#2235 = ORIENTED_EDGE ( 'NONE', *, *, #3215, .T. ) ;
#2236 = CARTESIAN_POINT ( 'NONE',  ( -21.18131961722757595, -44.04859572486944330, -1.453139578080854699 ) ) ;
#2237 = PRODUCT_RELATED_PRODUCT_CATEGORY ( 'part', '', ( #1628 ) ) ;
#2238 = CARTESIAN_POINT ( 'NONE',  ( -28.46154767013959486, -47.79859572486944330, 9.374751783755112200 ) ) ;
#2239 = CARTESIAN_POINT ( 'NONE',  ( -25.99212434019154472, -33.65140427513057375, 7.988596311142242890 ) ) ;
#2240 = ORIENTED_EDGE ( 'NONE', *, *, #7070, .T. ) ;
#2241 = CARTESIAN_POINT ( 'NONE',  ( -2.796473189345805913E-16, -40.43301269999997061, -100.2499999989075263 ) ) ;
#2242 = CARTESIAN_POINT ( 'NONE',  ( -25.68709025247441602, -30.60000000000000142, -8.464561979789547053 ) ) ;
#2243 = PLANE ( 'NONE',  #6295 ) ;
#2244 = CARTESIAN_POINT ( 'NONE',  ( 8.389419568037416259E-16, -49.56698729999997255, -96.84999999890752065 ) ) ;
#2245 = CARTESIAN_POINT ( 'NONE',  ( -26.64110105645932336, -7.999999999999996447, 124.0000000000000000 ) ) ;
#2246 = DIRECTION ( 'NONE',  ( 0.000000000000000000, 0.000000000000000000, 1.000000000000000000 ) ) ;
#2247 = EDGE_LOOP ( 'NONE', ( #8564, #6360 ) ) ;
#2248 = CARTESIAN_POINT ( 'NONE',  ( -23.95213185889994989, -41.49859572486943904, 5.972947139071243861 ) ) ;
#2249 = CARTESIAN_POINT ( 'NONE',  ( -20.13408869516453947, -40.05000000000001137, -1.562606840307983136 ) ) ;
#2250 = ORIENTED_EDGE ( 'NONE', *, *, #188, .F. ) ;
#2251 = CARTESIAN_POINT ( 'NONE',  ( -39.86591130483550671, -50.55000000000001137, 1.562606840307984468 ) ) ;
#2252 = DIRECTION ( 'NONE',  ( -0.000000000000000000, -0.000000000000000000, -1.000000000000000000 ) ) ;
#2253 = CARTESIAN_POINT ( 'NONE',  ( 42.00000000000000711, 48.00000000000002842, -20.34999999999992326 ) ) ;
#2254 = EDGE_CURVE ( 'NONE', #6385, #6416, #5740, .T. ) ;
#2255 = CARTESIAN_POINT ( 'NONE',  ( -2.071067811865475505, -49.99999999999996447, -98.74999999781503845 ) ) ;
#2256 = DIRECTION ( 'NONE',  ( 0.000000000000000000, 0.000000000000000000, 1.000000000000000000 ) ) ;
#2257 = CARTESIAN_POINT ( 'NONE',  ( -4.566987299999998307, -44.99999999999997158, -98.44999999890752918 ) ) ;
#2258 = ORIENTED_EDGE ( 'NONE', *, *, #1812, .T. ) ;
#2259 = CARTESIAN_POINT ( 'NONE',  ( -21.16389173201424612, -48.05140427513057233, -1.343104241417630185 ) ) ;
#2260 = CARTESIAN_POINT ( 'NONE',  ( 2.071067811865474173, -39.99999999999997158, -98.44300000002185413 ) ) ;
#2261 = CARTESIAN_POINT ( 'NONE',  ( 4.566987299999998307, -43.10829192115428299, -96.39999999890753202 ) ) ;
#2262 = CARTESIAN_POINT ( 'NONE',  ( -2.071067811865475505, -49.99999999999996447, -96.34999999781506119 ) ) ;
#2263 = VECTOR ( 'NONE', #5559, 1000.000000000000000 ) ;
#2264 = CARTESIAN_POINT ( 'NONE',  ( -41.99999999999996447, 60.00000000000002842, 23.64999999999999858 ) ) ;
#2265 = SHAPE_REPRESENTATION ( 'BR-006', ( #5360, #6353, #5802, #3556, #4244, #430, #2564, #571, #1860, #3133, #7484, #5650, #2432, #2995, #5508, #5098, #307 ), #171 ) ;
#2266 = ITEM_DEFINED_TRANSFORMATION ( 'NONE', 'NONE', #2432,  #2554 ) ;
#2267 = PRESENTATION_STYLE_ASSIGNMENT (( #3502 ) ) ;
#2268 = ADVANCED_FACE ( 'NONE', ( #3672 ), #1226, .T. ) ;
#2269 = CARTESIAN_POINT ( 'NONE',  ( -23.68028341417693738, -33.75000000000001421, -6.319716585823198507 ) ) ;
#2270 = CARTESIAN_POINT ( 'NONE',  ( 25.00000000000004263, -44.99999999999995737, 11.45643923738958314 ) ) ;
#2271 = DIRECTION ( 'NONE',  ( 1.000000000000000000, -0.000000000000000000, -0.000000000000000000 ) ) ;
#2272 = CARTESIAN_POINT ( 'NONE',  ( -28.43739315969223824, -33.45000000000000995, -9.865911304835512041 ) ) ;
#2273 = CARTESIAN_POINT ( 'NONE',  ( -2.071067811865475505, -49.99999999999997158, -98.04999999999999716 ) ) ;
#2274 = MECHANICAL_DESIGN_GEOMETRIC_PRESENTATION_REPRESENTATION (  '', ( #5499 ), #296 ) ;
#2275 = CARTESIAN_POINT ( 'NONE',  ( -20.13408869516454303, -40.05000000000001137, -1.562606840307982692 ) ) ;
#2276 = ORIENTED_EDGE ( 'NONE', *, *, #6083, .F. ) ;
#2277 = LINE ( 'NONE', #3144, #7975 ) ;
#2278 = ORIENTED_EDGE ( 'NONE', *, *, #8254, .F. ) ;
#2279 = CARTESIAN_POINT ( 'NONE',  ( -21.18131961722757595, -35.04859572486943620, -1.453139578080854699 ) ) ;
#2280 = CARTESIAN_POINT ( 'NONE',  ( -38.44051085762733777, -48.39859572486944472, 4.360112732550414982 ) ) ;
#2281 = CARTESIAN_POINT ( 'NONE',  ( -36.35910488754074521, -31.25140427513058228, 6.280328284105565650 ) ) ;
#2282 = CARTESIAN_POINT ( 'NONE',  ( 3.229347689422841228, -48.22934768942280925, -96.54999999890752349 ) ) ;
#2283 = DIRECTION ( 'NONE',  ( -1.000000000000000000, 0.000000000000000000, 0.000000000000000000 ) ) ;
#2284 = CARTESIAN_POINT ( 'NONE',  ( -34.83673358847238433, -43.69081521296089221, 11.52653374317613810 ) ) ;
#2285 = CARTESIAN_POINT ( 'NONE',  ( 4.566987299999998307, -43.10829192115428299, -98.99999999890751212 ) ) ;
#2286 = EDGE_CURVE ( 'NONE', #5578, #7382, #6687, .T. ) ;
#2287 = DIRECTION ( 'NONE',  ( 0.000000000000000000, 0.000000000000000000, -1.000000000000000000 ) ) ;
#2288 = CARTESIAN_POINT ( 'NONE',  ( 3.535533905932737309, -48.53553390593270933, -96.19999999781504130 ) ) ;
#2289 = DIRECTION ( 'NONE',  ( -1.000000000000000000, -0.000000000000000000, -0.000000000000000000 ) ) ;
#2290 = VERTEX_POINT ( 'NONE', #7013 ) ;
#2291 = CARTESIAN_POINT ( 'NONE',  ( -28.65689575858256077, -43.44859572486944188, -8.836108267985801845 ) ) ;
#2292 = CARTESIAN_POINT ( 'NONE',  ( -23.28248557872775137, -40.50000000000000711, 6.717514421272141156 ) ) ;
#2293 = APPLICATION_CONTEXT ( 'automotive_design' ) ;
#2294 = ORIENTED_EDGE ( 'NONE', *, *, #4818, .T. ) ;
#2295 = CONICAL_SURFACE ( 'NONE', #8620, 1.649999999999998579, 1.029744258676653645 ) ;
#2296 = CARTESIAN_POINT ( 'NONE',  ( -22.89739904353894318, -29.75140427513057517, -7.023824353025938549 ) ) ;
#2297 = FACE_OUTER_BOUND ( 'NONE', #8444, .T. ) ;
#2298 = CARTESIAN_POINT ( 'NONE',  ( -4.999999999999998224, -44.99999999999997158, -98.09999999781504698 ) ) ;
#2299 = CARTESIAN_POINT ( 'NONE',  ( -2.071067811865475505, -49.99999999999996447, -97.94999999781504130 ) ) ;
#2300 = DIRECTION ( 'NONE',  ( 1.000000000000000000, 0.000000000000000000, 0.000000000000000000 ) ) ;
#2301 = CARTESIAN_POINT ( 'NONE',  ( 1.891708078845685481, -49.56698729999997255, -97.39999999890751781 ) ) ;
#2302 = VERTEX_POINT ( 'NONE', #316 ) ;
#2303 = CARTESIAN_POINT ( 'NONE',  ( -36.35910488754074521, -49.25140427513058938, 6.280328284105565650 ) ) ;
#2304 = CIRCLE ( 'NONE', #5111, 9.999999999999994671 ) ;
#2305 = EDGE_CURVE ( 'NONE', #8625, #1907, #976, .T. ) ;
#2306 = CARTESIAN_POINT ( 'NONE',  ( 3.535533905932736420, -41.46446609406723383, -98.49300000002185129 ) ) ;
#2307 = CIRCLE ( 'NONE', #7360, 1.000000000000000888 ) ;
#2308 = CARTESIAN_POINT ( 'NONE',  ( -1.891708078845683039, -40.43301269999998482, -95.39999999890751781 ) ) ;
#2309 = AXIS2_PLACEMENT_3D ( 'NONE', #1256, #819, #2944 ) ;
#2310 = CARTESIAN_POINT ( 'NONE',  ( -3.535533905932736864, -41.46446609406723383, -95.79999999781504982 ) ) ;
#2311 = DIRECTION ( 'NONE',  ( -0.000000000000000000, -0.000000000000000000, -1.000000000000000000 ) ) ;
#2312 = CARTESIAN_POINT ( 'NONE',  ( -2.071067811865475505, -49.99999999999997158, -100.3499999978150612 ) ) ;
#2313 = EDGE_CURVE ( 'NONE', #1434, #120, #8639, .T. ) ;
#2314 = CARTESIAN_POINT ( 'NONE',  ( -38.82739432537914581, -38.54999999999999716, 1.398121909749243441 ) ) ;
#2315 = AXIS2_PLACEMENT_3D ( 'NONE', #2179, #2840, #141 ) ;
#2316 = CARTESIAN_POINT ( 'NONE',  ( 4.566987299999998307, -44.99999999999997158, -95.84999999890752065 ) ) ;
#2317 = CARTESIAN_POINT ( 'NONE',  ( -21.53543802021056663, -33.90000000000000568, -4.312909747525783821 ) ) ;
#2318 = VECTOR ( 'NONE', #5441, 1000.000000000000000 ) ;
#2319 = DIRECTION ( 'NONE',  ( -0.000000000000000000, 1.000000000000000000, -0.000000000000000000 ) ) ;
#2320 = CARTESIAN_POINT ( 'NONE',  ( -39.86591130483550671, -44.55000000000000426, 1.562606840307984690 ) ) ;
#2321 = ORIENTED_EDGE ( 'NONE', *, *, #1609, .T. ) ;
#2322 = CARTESIAN_POINT ( 'NONE',  ( -33.35889894354067309, 8.000000000000000000, 124.0000000000000000 ) ) ;
#2323 = VERTEX_POINT ( 'NONE', #2400 ) ;
#2324 = CARTESIAN_POINT ( 'NONE',  ( -36.28032828410546529, -42.24859572486943904, 6.359104887540839357 ) ) ;
#2325 = CARTESIAN_POINT ( 'NONE',  ( -38.92545601287626056, -48.84859572486942625, -4.485229520447501450 ) ) ;
#2326 = CARTESIAN_POINT ( 'NONE',  ( -34.00787565980851213, -32.15140427513058086, -7.988596311142238449 ) ) ;
#2327 = EDGE_CURVE ( 'NONE', #2012, #6772, #1293, .T. ) ;
#2328 = CARTESIAN_POINT ( 'NONE',  ( -4.566987299999998307, -44.99999999999997158, -99.24999999890752633 ) ) ;
#2329 = CARTESIAN_POINT ( 'NONE',  ( 31.31030599380072488, -40.16344083911685914, 12.43538147425379492 ) ) ;
#2330 = CARTESIAN_POINT ( 'NONE',  ( -34.31290974752564438, -32.10000000000000142, 8.464561979789547053 ) ) ;
#2331 = CARTESIAN_POINT ( 'NONE',  ( 1.891708078845685481, -49.56698729999997255, -97.59999999890754907 ) ) ;
#2332 = LINE ( 'NONE', #5668, #8235 ) ;
#2333 = CARTESIAN_POINT ( 'NONE',  ( 1.891708078845685481, -49.56698729999997255, -95.99999999890751212 ) ) ;
#2334 = ORIENTED_EDGE ( 'NONE', *, *, #1974, .T. ) ;
#2335 = CARTESIAN_POINT ( 'NONE',  ( -25.89286002894218086, -41.64859572486943762, 7.938018618334153231 ) ) ;
#2336 = CARTESIAN_POINT ( 'NONE',  ( -36.71751442127229836, -45.00000000000000711, -6.717514421272142044 ) ) ;
#2337 = EDGE_LOOP ( 'NONE', ( #21, #688 ) ) ;
#2338 = CARTESIAN_POINT ( 'NONE',  ( -25.51477047955235378, -30.65140427513057730, 8.925456012876139766 ) ) ;
#2339 = CARTESIAN_POINT ( 'NONE',  ( -4.999999999999998224, -42.92893218813449607, -96.54999999781504982 ) ) ;
#2340 = CARTESIAN_POINT ( 'NONE',  ( 3.229347689422841228, -48.22934768942280925, -99.94999999890752918 ) ) ;
#2341 = CARTESIAN_POINT ( 'NONE',  ( 4.999999999999998224, -42.92893218813448897, -98.44999999781505551 ) ) ;
#2342 = CARTESIAN_POINT ( 'NONE',  ( -30.00000000000000000, -49.99999999999997158, 0.000000000000000000 ) ) ;
#2343 = CARTESIAN_POINT ( 'NONE',  ( -2.071067811865475061, -39.99999999999997158, -95.95000000000003126 ) ) ;
#2344 = ORIENTED_EDGE ( 'NONE', *, *, #1018, .F. ) ;
#2345 = PRODUCT ( 'sliding jaw', 'sliding jaw', '', ( #6134 ) ) ;
#2346 = CARTESIAN_POINT ( 'NONE',  ( -21.60464910494133406, -31.20000000000000639, 1.329692952841886155 ) ) ;
#2347 = VECTOR ( 'NONE', #1550, 1000.000000000000000 ) ;
#2348 = EDGE_LOOP ( 'NONE', ( #6889, #2040, #6457 ) ) ;
#2349 = ADVANCED_FACE ( 'NONE', ( #1623 ), #3574, .F. ) ;
#2350 = CARTESIAN_POINT ( 'NONE',  ( -3.229347689422840784, -41.77065231057713390, -96.14999999890753202 ) ) ;
#2351 = CARTESIAN_POINT ( 'NONE',  ( -4.999999999999997335, -47.07106781186546129, -96.44999999781505551 ) ) ;
#2352 = LINE ( 'NONE', #4945, #3676 ) ;
#2353 = ITEM_DEFINED_TRANSFORMATION ( 'NONE', 'NONE', #7484,  #2554 ) ;
#2354 = AXIS2_PLACEMENT_3D ( 'NONE', #2982, #3512, #6476 ) ;
#2355 = FACE_OUTER_BOUND ( 'NONE', #3951, .T. ) ;
#2356 = CARTESIAN_POINT ( 'NONE',  ( -31.32969295284206979, -36.30000000000000426, -8.395350895058669494 ) ) ;
#2357 = CONICAL_SURFACE ( 'NONE', #3061, 1.649999999999998579, 1.029744258676653645 ) ;
#2358 = CARTESIAN_POINT ( 'NONE',  ( -3.229347689422839451, -48.22934768942280925, -96.14999999890753202 ) ) ;
#2359 = CARTESIAN_POINT ( 'NONE',  ( -3.535533905932736864, -41.46446609406723383, -98.29999999999999716 ) ) ;
#2360 = CARTESIAN_POINT ( 'NONE',  ( -21.53543802021056663, -30.90000000000000924, -4.312909747525783821 ) ) ;
#2361 = EDGE_CURVE ( 'NONE', #6150, #858, #7319, .T. ) ;
#2362 = DIRECTION ( 'NONE',  ( -1.000000000000000000, 0.000000000000000000, 0.000000000000000000 ) ) ;
#2363 = CARTESIAN_POINT ( 'NONE',  ( -25.46513832392766119, -37.65000000000000568, 8.900167166472096270 ) ) ;
#2364 = CIRCLE ( 'NONE', #506, 10.00000000000000178 ) ;
#2365 = SHAPE_REPRESENTATION_RELATIONSHIP ( 'NONE' , 'NONE' ,  #7373, #7808 ) ;
#2366 = ORIENTED_EDGE ( 'NONE', *, *, #3395, .T. ) ;
#2367 = ORIENTED_EDGE ( 'NONE', *, *, #8442, .F. ) ;
#2368 = CARTESIAN_POINT ( 'NONE',  ( -25.89286002894218086, -35.64859572486943051, 7.938018618334153231 ) ) ;
#2369 = CARTESIAN_POINT ( 'NONE',  ( -28.46154767013959486, -44.79859572486943620, 9.374751783755112200 ) ) ;
#2370 = CARTESIAN_POINT ( 'NONE',  ( -31.45313957808072303, -33.95140427513058512, 8.818680382772479120 ) ) ;
#2371 = EDGE_CURVE ( 'NONE', #1415, #2848, #1002, .T. ) ;
#2372 = AXIS2_PLACEMENT_3D ( 'NONE', #7189, #358, #7108 ) ;
#2373 = CARTESIAN_POINT ( 'NONE',  ( -3.229347689422839451, -48.22934768942280925, -99.94999999890752918 ) ) ;
#2374 = DIRECTION ( 'NONE',  ( -0.000000000000000000, -0.000000000000000000, -1.000000000000000000 ) ) ;
#2375 = CARTESIAN_POINT ( 'NONE',  ( -23.28248557872775137, -40.50000000000000711, 6.717514421272141156 ) ) ;
#2376 = CARTESIAN_POINT ( 'NONE',  ( -1.891708078845683483, -49.56698729999997255, -100.0999999989075206 ) ) ;
#2377 = CARTESIAN_POINT ( 'NONE',  ( -26.69235372381821847, -48.76359959685383672, 12.05680772549333923 ) ) ;
#2378 = CARTESIAN_POINT ( 'NONE',  ( -1.891708078845683483, -49.56698729999997255, -97.69999999890751496 ) ) ;
#2379 = EDGE_CURVE ( 'NONE', #8500, #6529, #6337, .T. ) ;
#2380 = ORIENTED_EDGE ( 'NONE', *, *, #7605, .T. ) ;
#2381 = CARTESIAN_POINT ( 'NONE',  ( -25.89286002894218086, -44.64859572486944472, 7.938018618334153231 ) ) ;
#2382 = CARTESIAN_POINT ( 'NONE',  ( -39.86591130483550671, -47.54999999999999716, 1.562606840307984468 ) ) ;
#2383 = ADVANCED_FACE ( 'NONE', ( #4932 ), #2958, .T. ) ;
#2384 = ORIENTED_EDGE ( 'NONE', *, *, #8442, .T. ) ;
#2385 = CARTESIAN_POINT ( 'NONE',  ( -28.56619749409589204, -36.80140427513057944, 9.391326687552490782 ) ) ;
#2386 = DIRECTION ( 'NONE',  ( 1.000000000000000000, 0.000000000000000000, 0.000000000000000000 ) ) ;
#2387 = CARTESIAN_POINT ( 'NONE',  ( 4.999999999999994671, -42.92893218813449607, -98.44999999781506972 ) ) ;
#2388 = CARTESIAN_POINT ( 'NONE',  ( -50.00000000000002842, -44.99999999999997158, -2.099999999999997868 ) ) ;
#2389 = CARTESIAN_POINT ( 'NONE',  ( -4.999999999999998224, -44.99999999999997158, -96.49999999781503845 ) ) ;
#2390 = CARTESIAN_POINT ( 'NONE',  ( -1.891708078845683039, -40.43301269999998482, -100.1999999989075150 ) ) ;
#2391 = ORIENTED_EDGE ( 'NONE', *, *, #8234, .T. ) ;
#2392 = CARTESIAN_POINT ( 'NONE',  ( -26.14108075221394856, -36.60000000000000853, -7.573555455601170827 ) ) ;
#2393 = EDGE_LOOP ( 'NONE', ( #5113, #4384, #5262, #7550 ) ) ;
#2394 = CARTESIAN_POINT ( 'NONE',  ( 3.535533905932737309, -48.53553390593270933, -97.10000000000000853 ) ) ;
#2395 = EDGE_CURVE ( 'NONE', #1100, #724, #919, .T. ) ;
#2396 = CARTESIAN_POINT ( 'NONE',  ( -33.35889894354067309, -7.999999999999996447, 124.0000000000000000 ) ) ;
#2397 = DIRECTION ( 'NONE',  ( -1.000000000000000000, -0.000000000000000000, -0.000000000000000000 ) ) ;
#2398 = CARTESIAN_POINT ( 'NONE',  ( -38.82739432537914581, -44.55000000000001137, 1.398121909749243441 ) ) ;
#2399 = DIRECTION ( 'NONE',  ( 0.000000000000000000, 0.000000000000000000, -1.000000000000000000 ) ) ;
#2400 = CARTESIAN_POINT ( 'NONE',  ( 39.85000000000002274, -21.99999999999992184, 80.00000000000002842 ) ) ;
#2401 = AXIS2_PLACEMENT_3D ( 'NONE', #5782, #433, #1024 ) ;
#2402 = DIRECTION ( 'NONE',  ( -1.000000000000000000, 0.000000000000000000, 0.000000000000000000 ) ) ;
#2403 = CARTESIAN_POINT ( 'NONE',  ( -34.53486167607238144, -36.15000000000001279, -8.900167166472096270 ) ) ;
#2404 = CARTESIAN_POINT ( 'NONE',  ( -39.84999999999998010, 22.00000000000000000, 60.00000000000002842 ) ) ;
#2405 = CARTESIAN_POINT ( 'NONE',  ( -39.86591130483550671, -38.55000000000000426, 1.562606840307984690 ) ) ;
#2406 = ORIENTED_EDGE ( 'NONE', *, *, #3223, .F. ) ;
#2407 = CARTESIAN_POINT ( 'NONE',  ( -37.98859631114233792, -48.84859572486942625, -4.007875659808334490 ) ) ;
#2408 = CARTESIAN_POINT ( 'NONE',  ( -36.71751442127229836, -30.00000000000000711, -6.717514421272142044 ) ) ;
#2409 = CARTESIAN_POINT ( 'NONE',  ( -31.45313957808072303, -36.95140427513057801, 8.818680382772479120 ) ) ;
#2410 = CIRCLE ( 'NONE', #5487, 1.000000000000000888 ) ;
#2411 = ADVANCED_FACE ( 'NONE', ( #3614 ), #7529, .T. ) ;
#2412 = LINE ( 'NONE', #3809, #5727 ) ;
#2413 = DIRECTION ( 'NONE',  ( 1.000000000000000000, 0.000000000000000000, 0.000000000000000000 ) ) ;
#2414 = CARTESIAN_POINT ( 'NONE',  ( -39.38303923565386100, -41.70000000000000995, -1.486127417882099788 ) ) ;
#2415 = CARTESIAN_POINT ( 'NONE',  ( 3.229347689422839895, -41.77065231057713390, -99.74999999890751212 ) ) ;
#2416 = LINE ( 'NONE', #1081, #605 ) ;
#2417 = CARTESIAN_POINT ( 'NONE',  ( -3.229347689422840784, -41.77065231057713390, -96.34999999890752065 ) ) ;
#2418 = VERTEX_POINT ( 'NONE', #5677 ) ;
#2419 = CARTESIAN_POINT ( 'NONE',  ( -41.99999999999996447, 47.00857997860455129, 22.00000000000000000 ) ) ;
#2420 = CARTESIAN_POINT ( 'NONE',  ( -36.28032828410546529, -39.24859572486943904, 6.359104887540839357 ) ) ;
#2421 = CARTESIAN_POINT ( 'NONE',  ( -21.53543802021056663, -48.90000000000000568, -4.312909747525783821 ) ) ;
#2422 = VERTEX_POINT ( 'NONE', #213 ) ;
#2423 = CARTESIAN_POINT ( 'NONE',  ( -22.89739904353894318, -35.75140427513057517, -7.023824353025938549 ) ) ;
#2424 = DIRECTION ( 'NONE',  ( -0.000000000000000000, -0.000000000000000000, -1.000000000000000000 ) ) ;
#2425 = CARTESIAN_POINT ( 'NONE',  ( -33.35889894354067309, 9.000000000000001776, 125.0000000000000000 ) ) ;
#2426 = DIRECTION ( 'NONE',  ( -0.000000000000000000, -0.000000000000000000, -1.000000000000000000 ) ) ;
#2427 = STYLED_ITEM ( 'NONE', ( #6012 ), #2772 ) ;
#2428 = CARTESIAN_POINT ( 'NONE',  ( 0.000000000000000000, 0.000000000000000000, 1.622657008870242981E-16 ) ) ;
#2429 = CARTESIAN_POINT ( 'NONE',  ( 5.000000000000000000, -47.07106781186545419, -96.25000000000000000 ) ) ;
#2430 = ORIENTED_EDGE ( 'NONE', *, *, #188, .T. ) ;
#2431 = CARTESIAN_POINT ( 'NONE',  ( -21.17260567462091458, -34.04999999999998295, -1.398121909749242331 ) ) ;
#2432 = AXIS2_PLACEMENT_3D ( 'NONE', #4505, #7192, #1151 ) ;
#2433 = ORIENTED_EDGE ( 'NONE', *, *, #818, .T. ) ;
#2434 = CARTESIAN_POINT ( 'NONE',  ( 4.999999999999998224, -42.92893218813448897, -96.15000000000000568 ) ) ;
#2435 = CARTESIAN_POINT ( 'NONE',  ( -4.999999999999998224, -42.92893218813448897, -98.14999999781504414 ) ) ;
#2436 = AXIS2_PLACEMENT_3D ( 'NONE', #128, #1581, #7531 ) ;
#2437 = CARTESIAN_POINT ( 'NONE',  ( -30.00000000000000000, 0.000000000000000000, 60.00000000000002842 ) ) ;
#2438 = CONTEXT_DEPENDENT_SHAPE_REPRESENTATION ( #5153, #7578 ) ;
#2439 = DIRECTION ( 'NONE',  ( -1.000000000000000000, -0.000000000000000000, -0.000000000000000000 ) ) ;
#2440 = AXIS2_PLACEMENT_3D ( 'NONE', #501, #3826, #7091 ) ;
#2441 = DIRECTION ( 'NONE',  ( 0.000000000000000000, 0.000000000000000000, -1.000000000000000000 ) ) ;
#2442 = CARTESIAN_POINT ( 'NONE',  ( 44.14999999999999147, -21.99999999999992184, 80.00000000000002842 ) ) ;
#2443 = CARTESIAN_POINT ( 'NONE',  ( 0.000000000000000000, -1.773042676681341634, 2.493664996716660198E-15 ) ) ;
#2444 = LINE ( 'NONE', #1149, #5034 ) ;
#2445 = CARTESIAN_POINT ( 'NONE',  ( -38.90016716647221529, -38.85000000000000853, -4.534861676072185155 ) ) ;
#2446 = CIRCLE ( 'NONE', #1030, 9.999999999999994671 ) ;
#2447 = ORIENTED_EDGE ( 'NONE', *, *, #4575, .F. ) ;
#2448 = CARTESIAN_POINT ( 'NONE',  ( -22.45049566656107842, -46.89859572486944472, -3.906122232810846917 ) ) ;
#2449 = CARTESIAN_POINT ( 'NONE',  ( -25.68709025247441602, -33.60000000000000142, -8.464561979789547053 ) ) ;
#2450 = CARTESIAN_POINT ( 'NONE',  ( -38.83610826798580717, -37.55140427513057944, 1.343104241417631073 ) ) ;
#2451 = CARTESIAN_POINT ( 'NONE',  ( 4.566987299999998307, -44.99999999999997158, -98.84999999890753486 ) ) ;
#2452 = CARTESIAN_POINT ( 'NONE',  ( 25.00000000000003553, -45.33027059730881092, 11.45643923738957781 ) ) ;
#2453 = CARTESIAN_POINT ( 'NONE',  ( -21.09983283352784156, -37.35000000000000853, 4.534861676072186043 ) ) ;
#2454 = LINE ( 'NONE', #7202, #2119 ) ;
#2455 = LINE ( 'NONE', #7651, #1759 ) ;
#2456 = CARTESIAN_POINT ( 'NONE',  ( -2.796473189345805913E-16, -40.43301269999997061, -98.04999999890752349 ) ) ;
#2457 = DIRECTION ( 'NONE',  ( 0.000000000000000000, 0.4999999999999989453, -0.8660254037844392627 ) ) ;
#2458 = ORIENTED_EDGE ( 'NONE', *, *, #6769, .T. ) ;
#2459 = CARTESIAN_POINT ( 'NONE',  ( -38.92545601287626056, -33.84859572486942625, -4.485229520447501450 ) ) ;
#2460 = CARTESIAN_POINT ( 'NONE',  ( -31.61762450863942320, -30.95140427513058157, 9.857197362228843573 ) ) ;
#2461 = EDGE_CURVE ( 'NONE', #7413, #7480, #5633, .T. ) ;
#2462 = ORIENTED_EDGE ( 'NONE', *, *, #395, .F. ) ;
#2463 = CARTESIAN_POINT ( 'NONE',  ( -39.37475178375516549, -37.70140427513057091, -1.538452329860249712 ) ) ;
#2464 = CARTESIAN_POINT ( 'NONE',  ( -33.31087205654255712, -48.76061935842974293, 12.05589577412332680 ) ) ;
#2465 = CARTESIAN_POINT ( 'NONE',  ( -30.00000000000002487, 0.000000000000000000, -29.65000000000000213 ) ) ;
#2466 = CARTESIAN_POINT ( 'NONE',  ( -2.071067811865475505, -49.99999999999997158, -97.25000000000000000 ) ) ;
#2467 = CARTESIAN_POINT ( 'NONE',  ( -41.99999999999996447, 48.00000000000002842, -22.00000000000000000 ) ) ;
#2468 = CARTESIAN_POINT ( 'NONE',  ( -2.796473189345805913E-16, -40.43301269999997061, -100.2499999989075263 ) ) ;
#2469 = ADVANCED_FACE ( 'NONE', ( #2916 ), #4304, .F. ) ;
#2470 = ORIENTED_EDGE ( 'NONE', *, *, #2478, .T. ) ;
#2471 = CARTESIAN_POINT ( 'NONE',  ( -33.85891924778610473, -38.10000000000000853, 7.573555455601171715 ) ) ;
#2472 = EDGE_CURVE ( 'NONE', #1354, #5482, #2908, .T. ) ;
#2473 = ORIENTED_EDGE ( 'NONE', *, *, #2678, .F. ) ;
#2474 = CARTESIAN_POINT ( 'NONE',  ( 4.999999999999998224, -44.99999999999997158, -96.20000000000000284 ) ) ;
#2475 = CARTESIAN_POINT ( 'NONE',  ( 4.921782859443697866, -45.92696902661836589, -99.99920284823379291 ) ) ;
#2476 = VECTOR ( 'NONE', #6589, 1000.000000000000000 ) ;
#2477 = B_SPLINE_CURVE_WITH_KNOTS ( 'NONE', 3,
 ( #2199, #4884, #4218, #205, #2907, #5576, #8284, #1121, #992, #2377, #1614, #5052, #4303, #7742, #5011, #2991, #4968, #1705 ),
 .UNSPECIFIED., .F., .F.,
 ( 4, 2, 2, 2, 2, 2, 2, 2, 4 ),
 ( 0.02369462427231873447, 0.02468136329545929375, 0.02566810231859985303, 0.02665484134174040884, 0.02764158036488096812, 0.02862831938802152740, 0.02961505841116208321, 0.03060179743430264249, 0.03158853645744320177 ),
 .UNSPECIFIED. ) ;
#2478 = EDGE_CURVE ( 'NONE', #7472, #4525, #7823, .T. ) ;
#2479 = DIRECTION ( 'NONE',  ( -1.000000000000000000, 0.000000000000000000, 0.000000000000000000 ) ) ;
#2480 = CYLINDRICAL_SURFACE ( 'NONE', #312, 2.149999999999985256 ) ;
#2481 = ADVANCED_FACE ( 'NONE', ( #7752 ), #1049, .F. ) ;
#2482 = CIRCLE ( 'NONE', #8120, 10.00000000000000000 ) ;
#2483 = CARTESIAN_POINT ( 'NONE',  ( 44.14999999999999147, 21.99999999999992184, 80.00000000000002842 ) ) ;
#2484 = LINE ( 'NONE', #5164, #6164 ) ;
#2485 = CARTESIAN_POINT ( 'NONE',  ( -31.56260684030781505, -49.95000000000000995, 9.865911304835508489 ) ) ;
#2486 = VERTEX_POINT ( 'NONE', #7882 ) ;
#2487 = CARTESIAN_POINT ( 'NONE',  ( -23.24502507771338600, -32.49859572486943904, 6.680053920257780220 ) ) ;
#2488 = CARTESIAN_POINT ( 'NONE',  ( -25.46513832392765408, -34.64999999999998437, 8.900167166472096270 ) ) ;
#2489 = CARTESIAN_POINT ( 'NONE',  ( -34.00787565980851213, -41.15140427513058086, -7.988596311142238449 ) ) ;
#2490 = EDGE_CURVE ( 'NONE', #2072, #2323, #4529, .T. ) ;
#2491 = CARTESIAN_POINT ( 'NONE',  ( -4.566987299999997418, -46.89170807884566017, -99.19999999890751496 ) ) ;
#2492 = CARTESIAN_POINT ( 'NONE',  ( 34.24325503137513493, -42.35030295949444934, 11.75814120956404629 ) ) ;
#2493 = CARTESIAN_POINT ( 'NONE',  ( -37.02382435302582309, -39.24859572486943904, 7.102600956461226467 ) ) ;
#2494 = CARTESIAN_POINT ( 'NONE',  ( -31.56260684030781505, -37.94999999999998153, 9.865911304835510265 ) ) ;
#2495 = CARTESIAN_POINT ( 'NONE',  ( -4.566987299999998307, -43.10829192115428299, -100.2999999989075093 ) ) ;
#2496 = EDGE_CURVE ( 'NONE', #923, #7483, #380, .T. ) ;
#2497 = DIRECTION ( 'NONE',  ( -0.000000000000000000, -0.000000000000000000, -1.000000000000000000 ) ) ;
#2498 = CARTESIAN_POINT ( 'NONE',  ( -2.796473189345805913E-16, -40.43301269999997061, -100.4499999989075292 ) ) ;
#2499 = PRESENTATION_STYLE_ASSIGNMENT (( #8533 ) ) ;
#2500 = EDGE_LOOP ( 'NONE', ( #1042, #7341, #4078, #1650, #6553, #5001 ) ) ;
#2501 = DIRECTION ( 'NONE',  ( 0.000000000000000000, -1.000000000000000000, 0.000000000000000000 ) ) ;
#2502 = CIRCLE ( 'NONE', #946, 1.000000000000000888 ) ;
#2503 = CARTESIAN_POINT ( 'NONE',  ( -25.89286002894218086, -47.64859572486945183, 7.938018618334153231 ) ) ;
#2504 = CARTESIAN_POINT ( 'NONE',  ( -36.68005392025794009, -35.00140427513057517, -6.754974922286504757 ) ) ;
#2505 = AXIS2_PLACEMENT_3D ( 'NONE', #5133, #5794, #4433 ) ;
#2506 = VERTEX_POINT ( 'NONE', #544 ) ;
#2507 = ORIENTED_EDGE ( 'NONE', *, *, #4845, .T. ) ;
#2508 = CARTESIAN_POINT ( 'NONE',  ( -37.10260095646111012, -37.25140427513058228, 7.023824353025939438 ) ) ;
#2509 = CARTESIAN_POINT ( 'NONE',  ( -33.97303272786269446, -48.05319586029032308, 11.85336373935253285 ) ) ;
#2510 = DIRECTION ( 'NONE',  ( -0.000000000000000000, 1.000000000000000000, -0.000000000000000000 ) ) ;
#2511 = CARTESIAN_POINT ( 'NONE',  ( 3.535533905932737309, -48.53553390593270933, -97.10000000000000853 ) ) ;
#2512 = LINE ( 'NONE', #3660, #4539 ) ;
#2513 = CARTESIAN_POINT ( 'NONE',  ( 2.071067811865477282, -49.99999999999996447, -96.35000000000000853 ) ) ;
#2514 = VERTEX_POINT ( 'NONE', #5897 ) ;
#2515 = AXIS2_PLACEMENT_3D ( 'NONE', #3841, #1063, #7813 ) ;
#2516 = CARTESIAN_POINT ( 'NONE',  ( -31.32969295284206979, -45.30000000000000426, -8.395350895058669494 ) ) ;
#2517 = VERTEX_POINT ( 'NONE', #8582 ) ;
#2518 = CARTESIAN_POINT ( 'NONE',  ( -3.535533905932735532, -48.53553390593270933, -98.10000000000000853 ) ) ;
#2519 = CARTESIAN_POINT ( 'NONE',  ( 3.812685264810825814, -48.24684725664164375, -100.0006756392447471 ) ) ;
#2520 = CARTESIAN_POINT ( 'NONE',  ( -26.09387776718931917, -29.60140427513057659, -7.549504333439021941 ) ) ;
#2521 = CARTESIAN_POINT ( 'NONE',  ( -41.99999999999996447, 48.00000000000002842, 23.64999999999999858 ) ) ;
#2522 = FACE_BOUND ( 'NONE', #2500, .T. ) ;
#2523 = CARTESIAN_POINT ( 'NONE',  ( -23.98959235991431171, -31.50000000000000711, 6.010407640085604797 ) ) ;
#2524 = CARTESIAN_POINT ( 'NONE',  ( 4.999999999999998224, -42.92893218813449607, -97.75000000000001421 ) ) ;
#2525 = CARTESIAN_POINT ( 'NONE',  ( -34.53486167607238855, -48.15000000000001279, -8.900167166472096270 ) ) ;
#2526 = EDGE_CURVE ( 'NONE', #5895, #3379, #1878, .T. ) ;
#2527 = DIRECTION ( 'NONE',  ( 0.000000000000000000, 0.000000000000000000, 1.000000000000000000 ) ) ;
#2528 = ORIENTED_EDGE ( 'NONE', *, *, #7148, .F. ) ;
#2529 = CARTESIAN_POINT ( 'NONE',  ( -38.40363834695740053, -48.69859572486944188, -1.277368040863739118 ) ) ;
#2530 = CARTESIAN_POINT ( 'NONE',  ( -31.48612741788231517, -33.30000000000000426, -9.383039235653804155 ) ) ;
#2531 = CARTESIAN_POINT ( 'NONE',  ( -36.35910488754074521, -37.25140427513058228, 6.280328284105565650 ) ) ;
#2532 = CARTESIAN_POINT ( 'NONE',  ( -20.00000000000002487, 0.000000000000000000, -44.00000000000000000 ) ) ;
#2533 = CARTESIAN_POINT ( 'NONE',  ( -41.99999999999996447, 48.00000000000002842, -22.00000000000000000 ) ) ;
#2534 = CARTESIAN_POINT ( 'NONE',  ( -23.24502507771338600, -41.49859572486943904, 6.680053920257780220 ) ) ;
#2535 = CARTESIAN_POINT ( 'NONE',  ( -31.48612741788231517, -39.30000000000001137, -9.383039235653804155 ) ) ;
#2536 = CARTESIAN_POINT ( 'NONE',  ( 4.566987300000000083, -46.89170807884565306, -99.89999999890751781 ) ) ;
#2537 = CARTESIAN_POINT ( 'NONE',  ( -33.35889894354067309, -8.999999999999998224, -24.00000000000000000 ) ) ;
#2538 = CARTESIAN_POINT ( 'NONE',  ( 4.566987300000000083, -46.89170807884565306, -99.89999999890751781 ) ) ;
#2539 = AXIS2_PLACEMENT_3D ( 'NONE', #7911, #8572, #4474 ) ;
#2540 = VERTEX_POINT ( 'NONE', #4403 ) ;
#2541 = DIRECTION ( 'NONE',  ( -0.000000000000000000, 1.000000000000000000, -0.000000000000000000 ) ) ;
#2542 =( BOUNDED_CURVE ( )  B_SPLINE_CURVE ( 2, ( #7712, #1765, #3175, #5063, #1050, #1717, #6465, #7883, #3742 ),
 .UNSPECIFIED., .F., .T. ) 
 B_SPLINE_CURVE_WITH_KNOTS ( ( 3, 2, 2, 2, 3 ),
 ( 0.2857142857142856984, 0.3035714285714285476, 0.3214285714285715079, 0.3392857142857143571, 0.3571428571428572063 ),
 .UNSPECIFIED. ) 
 CURVE ( )  GEOMETRIC_REPRESENTATION_ITEM ( )  RATIONAL_B_SPLINE_CURVE ( ( 1.000000000000000000, 0.9238795325112867385, 1.000000000000000000, 0.9238795325112867385, 1.000000000000000000, 0.9238795325112867385, 1.000000000000000000, 0.9238795325112865164, 1.000000000000000222 ) ) 
 REPRESENTATION_ITEM ( '' )  );
#2543 = CARTESIAN_POINT ( 'NONE',  ( -25.73429323749904185, -34.59859572486944046, -8.488613101951701267 ) ) ;
#2544 = CARTESIAN_POINT ( 'NONE',  ( -36.68005392025794009, -32.00140427513057517, -6.754974922286504757 ) ) ;
#2545 = EDGE_LOOP ( 'NONE', ( #6333, #1745, #2108, #1761 ) ) ;
#2546 = ORIENTED_EDGE ( 'NONE', *, *, #6773, .F. ) ;
#2547 = CARTESIAN_POINT ( 'NONE',  ( -39.87462524744216807, -31.55140427513057588, 1.507589171976367215 ) ) ;
#2548 = EDGE_CURVE ( 'NONE', #5875, #4340, #4411, .T. ) ;
#2549 = DIRECTION ( 'NONE',  ( -0.000000000000000000, -0.000000000000000000, -1.000000000000000000 ) ) ;
#2550 = CARTESIAN_POINT ( 'NONE',  ( 4.999999999999998224, -44.99999999999997158, -95.00000000000000000 ) ) ;
#2551 = CARTESIAN_POINT ( 'NONE',  ( 30.66531197710604317, -49.96635986460696444, 12.48644052906005264 ) ) ;
#2552 = CARTESIAN_POINT ( 'NONE',  ( 2.071067811865474173, -39.99999999999997158, -98.44999999999998863 ) ) ;
#2553 = ORIENTED_EDGE ( 'NONE', *, *, #3495, .F. ) ;
#2554 = AXIS2_PLACEMENT_3D ( 'NONE', #7787, #1707, #3692 ) ;
#2555 = CARTESIAN_POINT ( 'NONE',  ( -34.05750781543318340, -45.14999999999999858, -7.963307464738195840 ) ) ;
#2556 = STYLED_ITEM ( 'NONE', ( #4564 ), #24 ) ;
#2557 = EDGE_LOOP ( 'NONE', ( #3044, #8114, #7247, #3662 ) ) ;
#2558 = DIRECTION ( 'NONE',  ( -0.8660254037844382635, 0.000000000000000000, 0.5000000000000005551 ) ) ;
#2559 = CARTESIAN_POINT ( 'NONE',  ( -2.071067811865475505, -49.99999999999996447, -96.45000000000000284 ) ) ;
#2560 = CARTESIAN_POINT ( 'NONE',  ( -36.71751442127229836, -42.00000000000000711, -6.717514421272142044 ) ) ;
#2561 = CARTESIAN_POINT ( 'NONE',  ( -4.566987299999997418, -46.89170807884566727, -99.19999999890751496 ) ) ;
#2562 = CARTESIAN_POINT ( 'NONE',  ( 3.425853254208287346, -48.65268606878520075, -99.99975844170711525 ) ) ;
#2563 = CARTESIAN_POINT ( 'NONE',  ( -22.40239342223677355, -32.90140427513058086, -3.811716262761597473 ) ) ;
#2564 = AXIS2_PLACEMENT_3D ( 'NONE', #7234, #5284, #3977 ) ;
#2565 = EDGE_CURVE ( 'NONE', #1072, #5184, #3012, .T. ) ;
#2566 =( REPRESENTATION_RELATIONSHIP ('NONE','NONE', #2265, #3450 ) REPRESENTATION_RELATIONSHIP_WITH_TRANSFORMATION ( #7498 )SHAPE_REPRESENTATION_RELATIONSHIP( ) );
#2567 = AXIS2_PLACEMENT_3D ( 'NONE', #381, #8504, #8465 ) ;
#2568 = DIRECTION ( 'NONE',  ( -1.000000000000000000, 0.000000000000000000, -0.000000000000000000 ) ) ;
#2569 = VECTOR ( 'NONE', #3829, 1000.000000000000000 ) ;
#2570 = CARTESIAN_POINT ( 'NONE',  ( -33.85891924778610473, -32.10000000000000142, 7.573555455601171715 ) ) ;
#2571 = CARTESIAN_POINT ( 'NONE',  ( -4.999999999999998224, -44.99999999999997158, -97.40000000000000568 ) ) ;
#2572 = CARTESIAN_POINT ( 'NONE',  ( -30.00000000000002842, 0.000000000000000000, -40.35000000000000142 ) ) ;
#2573 = EDGE_CURVE ( 'NONE', #5405, #3069, #1848, .T. ) ;
#2574 = EDGE_CURVE ( 'NONE', #764, #4208, #7785, .T. ) ;
#2575 = DIRECTION ( 'NONE',  ( -1.000000000000000000, 0.000000000000000000, 0.000000000000000000 ) ) ;
#2576 = ORIENTED_EDGE ( 'NONE', *, *, #1539, .T. ) ;
#2577 = CARTESIAN_POINT ( 'NONE',  ( -37.54950433343896776, -51.39859572486944472, 3.906122232810848249 ) ) ;
#2578 = CARTESIAN_POINT ( 'NONE',  ( -38.46456197978948666, -32.40000000000000568, 4.312909747525784709 ) ) ;
#2579 = AXIS2_PLACEMENT_3D ( 'NONE', #8632, #2065, #1891 ) ;
#2580 = CARTESIAN_POINT ( 'NONE',  ( -37.93801861833426159, -40.85140427513057659, -4.107139971057695682 ) ) ;
#2581 = CARTESIAN_POINT ( 'NONE',  ( -26.64110105645932336, 9.000000000000001776, 125.0000000000000000 ) ) ;
#2582 = CARTESIAN_POINT ( 'NONE',  ( 0.000000000000000000, -44.99999999999997158, -105.0000000000000142 ) ) ;
#2583 = CARTESIAN_POINT ( 'NONE',  ( -36.75497492228666374, -36.99859572486943193, -6.680053920257780220 ) ) ;
#2584 = CARTESIAN_POINT ( 'NONE',  ( -21.09983283352784156, -43.35000000000000853, 4.534861676072186043 ) ) ;
#2585 = DIRECTION ( 'NONE',  ( 0.000000000000000000, 1.000000000000000000, 0.000000000000000000 ) ) ;
#2586 = DIRECTION ( 'NONE',  ( 0.000000000000000000, 0.000000000000000000, 1.000000000000000000 ) ) ;
#2587 = CARTESIAN_POINT ( 'NONE',  ( 1.891708078845682595, -40.43301269999998482, -99.69999999890752918 ) ) ;
#2588 = ORIENTED_EDGE ( 'NONE', *, *, #1822, .F. ) ;
#2589 = CARTESIAN_POINT ( 'NONE',  ( -30.00000000000000000, 60.00000000000002842, 12.49999999999998046 ) ) ;
#2590 = ADVANCED_FACE ( 'NONE', ( #8463 ), #6464, .T. ) ;
#2591 = CARTESIAN_POINT ( 'NONE',  ( -31.53845232986046554, -31.29859572486943975, -9.374751783755117529 ) ) ;
#2592 = CARTESIAN_POINT ( 'NONE',  ( -22.89739904353894318, -35.75140427513057517, -7.023824353025938549 ) ) ;
#2593 = ORIENTED_EDGE ( 'NONE', *, *, #8199, .F. ) ;
#2594 = VERTEX_POINT ( 'NONE', #7923 ) ;
#2595 = CARTESIAN_POINT ( 'NONE',  ( -20.12537475255788522, -48.05140427513057233, -1.507589171976365439 ) ) ;
#2596 = SURFACE_STYLE_USAGE ( .BOTH. , #1344 ) ;
#2597 = DIRECTION ( 'NONE',  ( -0.000000000000000000, -0.000000000000000000, 1.000000000000000000 ) ) ;
#2598 = CARTESIAN_POINT ( 'NONE',  ( 4.999999999999998224, -44.99999999999997158, -100.0999999978150470 ) ) ;
#2599 = DIRECTION ( 'NONE',  ( 0.000000000000000000, -0.000000000000000000, -1.000000000000000000 ) ) ;
#2600 = CARTESIAN_POINT ( 'NONE',  ( -50.00000000000002842, -30.00000000000000000, 80.00000000000002842 ) ) ;
#2601 = CIRCLE ( 'NONE', #8645, 1.000000000000000888 ) ;
#2602 = VERTEX_POINT ( 'NONE', #1889 ) ;
#2603 = CARTESIAN_POINT ( 'NONE',  ( -37.96330746473829976, -41.84999999999999432, -4.057507815433013754 ) ) ;
#2604 = ORIENTED_EDGE ( 'NONE', *, *, #275, .F. ) ;
#2605 = CARTESIAN_POINT ( 'NONE',  ( -4.566987299999998307, -44.99999999999997158, -95.44999999890751496 ) ) ;
#2606 = CARTESIAN_POINT ( 'NONE',  ( -3.061616997868382155E-16, -39.99999999999997158, -100.0000000000000000 ) ) ;
#2607 = CARTESIAN_POINT ( 'NONE',  ( -23.28248557872775137, -40.50000000000000711, 6.717514421272141156 ) ) ;
#2608 = CARTESIAN_POINT ( 'NONE',  ( -3.229347689422839451, -48.22934768942280925, -98.34999999890753486 ) ) ;
#2609 = CARTESIAN_POINT ( 'NONE',  ( -0.8026348516553690748, -49.96717851360725149, -99.99887219979210329 ) ) ;
#2610 = CARTESIAN_POINT ( 'NONE',  ( -24.02705286092866643, -30.50140427513058583, 6.047868141099968398 ) ) ;
#2611 = EDGE_CURVE ( 'NONE', #4408, #112, #8629, .T. ) ;
#2612 = CARTESIAN_POINT ( 'NONE',  ( 5.000000000000000000, -47.07106781186545419, -95.44300000002185413 ) ) ;
#2613 = CARTESIAN_POINT ( 'NONE',  ( -23.98959235991431171, -40.50000000000000711, 6.010407640085604797 ) ) ;
#2614 = DIRECTION ( 'NONE',  ( 0.000000000000000000, 0.000000000000000000, 1.000000000000000000 ) ) ;
#2615 = CARTESIAN_POINT ( 'NONE',  ( -25.46513832392766119, -46.65000000000001279, 8.900167166472096270 ) ) ;
#2616 = CARTESIAN_POINT ( 'NONE',  ( 0.000000000000000000, 0.000000000000000000, 0.000000000000000000 ) ) ;
#2617 = VERTEX_POINT ( 'NONE', #3741 ) ;
#2618 = FACE_BOUND ( 'NONE', #8172, .T. ) ;
#2619 = CARTESIAN_POINT ( 'NONE',  ( -28.43739315969223824, -42.44999999999999574, -9.865911304835512041 ) ) ;
#2620 = CARTESIAN_POINT ( 'NONE',  ( -21.60464910494133406, -31.20000000000000639, 1.329692952841886155 ) ) ;
#2621 = EDGE_CURVE ( 'NONE', #7038, #4958, #7171, .T. ) ;
#2622 = FACE_BOUND ( 'NONE', #7527, .T. ) ;
#2623 = PLANE ( 'NONE',  #7136 ) ;
#2624 = CARTESIAN_POINT ( 'NONE',  ( -39.39132668755255651, -39.69859572486944188, -1.433802505903950308 ) ) ;
#2625 = DIRECTION ( 'NONE',  ( 0.000000000000000000, 0.000000000000000000, 1.000000000000000000 ) ) ;
#2626 = FACE_OUTER_BOUND ( 'NONE', #7846, .T. ) ;
#2627 = CARTESIAN_POINT ( 'NONE',  ( -3.229347689422839451, -48.22934768942280925, -100.1499999989075178 ) ) ;
#2628 =( NAMED_UNIT ( * ) SI_UNIT ( $, .STERADIAN. ) SOLID_ANGLE_UNIT ( ) );
#2629 = ORIENTED_EDGE ( 'NONE', *, *, #911, .F. ) ;
#2630 = PLANE ( 'NONE',  #6651 ) ;
#2631 = CARTESIAN_POINT ( 'NONE',  ( -25.89286002894218086, -32.64859572486943762, 7.938018618334153231 ) ) ;
#2632 = CARTESIAN_POINT ( 'NONE',  ( -28.61798213517984024, -50.79859572486945041, 8.387063443159973986 ) ) ;
#2633 = CARTESIAN_POINT ( 'NONE',  ( -23.31994607974211675, -36.50140427513057517, 6.754974922286503869 ) ) ;
#2634 = CIRCLE ( 'NONE', #86, 12.00000000000004263 ) ;
#2635 = ORIENTED_EDGE ( 'NONE', *, *, #7694, .F. ) ;
#2636 = ORIENTED_EDGE ( 'NONE', *, *, #6281, .F. ) ;
#2637 = CARTESIAN_POINT ( 'NONE',  ( -21.12512167993187973, -45.35140427513057659, 4.584493831696868860 ) ) ;
#2638 = EDGE_CURVE ( 'NONE', #7971, #3466, #6506, .T. ) ;
#2639 =( NAMED_UNIT ( * ) PLANE_ANGLE_UNIT ( ) SI_UNIT ( $, .RADIAN. ) );
#2640 = CARTESIAN_POINT ( 'NONE',  ( 3.535533905932736420, -41.46446609406723383, -99.29999999999999716 ) ) ;
#2641 = CARTESIAN_POINT ( 'NONE',  ( 3.535533905932736420, -41.46446609406723383, -99.19999999781505551 ) ) ;
#2642 = CARTESIAN_POINT ( 'NONE',  ( -34.35889894354067309, -8.999999999999998224, 125.0000000000000000 ) ) ;
#2643 = CARTESIAN_POINT ( 'NONE',  ( -3.535533905932736864, -41.46446609406723383, -98.29999999999999716 ) ) ;
#2644 = ORIENTED_EDGE ( 'NONE', *, *, #916, .F. ) ;
#2645 = VECTOR ( 'NONE', #8366, 1000.000000000000114 ) ;
#2646 = EDGE_CURVE ( 'NONE', #3069, #2617, #7256, .T. ) ;
#2647 = CARTESIAN_POINT ( 'NONE',  ( -36.01040764008574513, -39.00000000000000711, -6.010407640085605685 ) ) ;
#2648 = VECTOR ( 'NONE', #3699, 1000.000000000000000 ) ;
#2649 = AXIS2_PLACEMENT_3D ( 'NONE', #7988, #1192, #4020 ) ;
#2650 = ORIENTED_EDGE ( 'NONE', *, *, #5685, .T. ) ;
#2651 = CARTESIAN_POINT ( 'NONE',  ( -3.229347689422839451, -48.22934768942280925, -96.94999999890751496 ) ) ;
#2652 = CARTESIAN_POINT ( 'NONE',  ( -4.999999999999998224, -44.99999999999997158, -95.69999999781504130 ) ) ;
#2653 = CARTESIAN_POINT ( 'NONE',  ( -25.68709025247441602, -48.60000000000000142, -8.464561979789547053 ) ) ;
#2654 = CARTESIAN_POINT ( 'NONE',  ( -4.566987299999997418, -46.89170807884566727, -99.99999999890754054 ) ) ;
#2655 = CARTESIAN_POINT ( 'NONE',  ( 4.999999999999998224, -44.99999999999997158, -95.00000000000000000 ) ) ;
#2656 = CARTESIAN_POINT ( 'NONE',  ( -31.27736804086391942, -29.30140427513058299, -8.403638346957361449 ) ) ;
#2657 = ADVANCED_BREP_SHAPE_REPRESENTATION ( '', ( #2810, #2554 ), #5211 ) ;
#2658 = CARTESIAN_POINT ( 'NONE',  ( -4.999999999999998224, -44.99999999999997158, -95.79300000002184845 ) ) ;
#2659 = CARTESIAN_POINT ( 'NONE',  ( -37.57355545560112375, -35.40000000000000568, 3.858919247786223305 ) ) ;
#2660 = DIRECTION ( 'NONE',  ( -0.000000000000000000, -0.000000000000000000, -1.000000000000000000 ) ) ;
#2661 = CYLINDRICAL_SURFACE ( 'NONE', #4685, 4.999999999999969802 ) ;
#2662 = DIRECTION ( 'NONE',  ( 0.000000000000000000, 0.000000000000000000, 1.000000000000000000 ) ) ;
#2663 = ORIENTED_EDGE ( 'NONE', *, *, #2951, .F. ) ;
#2664 = DIRECTION ( 'NONE',  ( 1.000000000000000000, 0.000000000000000000, 0.000000000000000000 ) ) ;
#2665 = CARTESIAN_POINT ( 'NONE',  ( -34.53486167607238144, -42.15000000000001279, -8.900167166472096270 ) ) ;
#2666 = CARTESIAN_POINT ( 'NONE',  ( -33.90612223281073057, -49.10140427513058370, 7.549504333439023718 ) ) ;
#2667 = CARTESIAN_POINT ( 'NONE',  ( 0.000000000000000000, 0.000000000000000000, 80.00000000000002842 ) ) ;
#2668 = CARTESIAN_POINT ( 'NONE',  ( -4.999999999999998224, -44.99999999999997158, -95.00000000000000000 ) ) ;
#2669 = CARTESIAN_POINT ( 'NONE',  ( -28.46154767013959486, -38.79859572486943620, 9.374751783755112200 ) ) ;
#2670 = CARTESIAN_POINT ( 'NONE',  ( -39.84999999999998010, -22.00000000000000000, 80.00000000000002842 ) ) ;
#2671 = LINE ( 'NONE', #6538, #5391 ) ;
#2672 = CARTESIAN_POINT ( 'NONE',  ( 3.229347689422841228, -48.22934768942280925, -95.74999999890752633 ) ) ;
#2673 = ORIENTED_EDGE ( 'NONE', *, *, #5647, .F. ) ;
#2674 = CARTESIAN_POINT ( 'NONE',  ( -26.64110105645932336, -7.999999999999996447, -25.00000000000000000 ) ) ;
#2675 = CARTESIAN_POINT ( 'NONE',  ( -33.81171626276147890, -33.09859572486943335, 7.597606577763319713 ) ) ;
#2676 = CARTESIAN_POINT ( 'NONE',  ( -22.97617564697422665, -40.74859572486943904, -7.102600956461224690 ) ) ;
#2677 = CARTESIAN_POINT ( 'NONE',  ( -34.48522952044771017, -41.15140427513058086, -8.925456012876139766 ) ) ;
#2678 = EDGE_CURVE ( 'NONE', #8357, #1249, #1217, .T. ) ;
#2679 = EDGE_LOOP ( 'NONE', ( #7568, #1238, #5361, #8662 ) ) ;
#2680 = EDGE_LOOP ( 'NONE', ( #738, #1950, #2716, #5385 ) ) ;
#2681 = CARTESIAN_POINT ( 'NONE',  ( -23.31994607974211675, -48.50140427513058938, 6.754974922286503869 ) ) ;
#2682 = CARTESIAN_POINT ( 'NONE',  ( -45.00000000000003553, -44.99999999999997158, 0.000000000000000000 ) ) ;
#2683 = DIRECTION ( 'NONE',  ( 0.000000000000000000, 0.000000000000000000, 1.000000000000000000 ) ) ;
#2684 = AXIS2_PLACEMENT_3D ( 'NONE', #7741, #7080, #446 ) ;
#2685 = CARTESIAN_POINT ( 'NONE',  ( 3.535533905932736420, -41.46446609406723383, -98.39999999781504414 ) ) ;
#2686 = CARTESIAN_POINT ( 'NONE',  ( 2.071067811865474173, -39.99999999999997158, -95.25000000000000000 ) ) ;
#2687 = FACE_OUTER_BOUND ( 'NONE', #4096, .T. ) ;
#2688 = ORIENTED_EDGE ( 'NONE', *, *, #4234, .T. ) ;
#2689 = CARTESIAN_POINT ( 'NONE',  ( -25.89286002894218086, -32.64859572486943762, 7.938018618334153231 ) ) ;
#2690 = CARTESIAN_POINT ( 'NONE',  ( -21.09983283352784156, -31.34999999999999787, 4.534861676072186043 ) ) ;
#2691 = VECTOR ( 'NONE', #4075, 1000.000000000000114 ) ;
#2692 = VERTEX_POINT ( 'NONE', #3254 ) ;
#2693 = CARTESIAN_POINT ( 'NONE',  ( -3.229347689422840784, -41.77065231057713390, -97.94999999890751496 ) ) ;
#2694 = CARTESIAN_POINT ( 'NONE',  ( 5.000000000000000000, -47.07106781186545419, -96.94999999781504130 ) ) ;
#2695 = AXIS2_PLACEMENT_3D ( 'NONE', #5625, #7449, #8119 ) ;
#2696 = CARTESIAN_POINT ( 'NONE',  ( -39.38303923565386100, -41.70000000000000995, -1.486127417882099788 ) ) ;
#2697 = CARTESIAN_POINT ( 'NONE',  ( 3.229347689422839895, -41.77065231057713390, -97.14999999890753202 ) ) ;
#2698 = CARTESIAN_POINT ( 'NONE',  ( -38.83610826798580717, -34.55140427513057233, 1.343104241417631073 ) ) ;
#2699 = EDGE_CURVE ( 'NONE', #598, #2752, #7129, .T. ) ;
#2700 = CARTESIAN_POINT ( 'NONE',  ( 9.184850993605145972E-16, -49.99999999999997158, -97.99300000002185129 ) ) ;
#2701 = CARTESIAN_POINT ( 'NONE',  ( -38.82739432537914581, -35.55000000000000426, 1.398121909749243663 ) ) ;
#2702 = LINE ( 'NONE', #1367, #4611 ) ;
#2703 = CARTESIAN_POINT ( 'NONE',  ( 2.000000000000000000, 1.880445160090761061E-16, -1.535500000000000087 ) ) ;
#2704 = CARTESIAN_POINT ( 'NONE',  ( -30.00000000000002842, 37.32500000000002416, 3.159706489353922981E-15 ) ) ;
#2705 = ORIENTED_EDGE ( 'NONE', *, *, #8170, .F. ) ;
#2706 = CARTESIAN_POINT ( 'NONE',  ( -3.535533905932735532, -48.53553390593270933, -99.70000000000000284 ) ) ;
#2707 = CARTESIAN_POINT ( 'NONE',  ( -36.71751442127229836, -42.00000000000000711, -6.717514421272142044 ) ) ;
#2708 = CARTESIAN_POINT ( 'NONE',  ( -26.14108075221394856, -30.60000000000000142, -7.573555455601170827 ) ) ;
#2709 = DIRECTION ( 'NONE',  ( -0.000000000000000000, 0.000000000000000000, -1.000000000000000000 ) ) ;
#2710 = CARTESIAN_POINT ( 'NONE',  ( -30.00000000000002487, 0.000000000000000000, -29.65000000000000213 ) ) ;
#2711 = CARTESIAN_POINT ( 'NONE',  ( -36.75497492228666374, -48.99859572486944614, -6.680053920257780220 ) ) ;
#2712 = DIRECTION ( 'NONE',  ( -0.000000000000000000, -0.000000000000000000, 1.000000000000000000 ) ) ;
#2713 = CARTESIAN_POINT ( 'NONE',  ( 9.184850993605145972E-16, -49.99999999999997158, -99.49999999781503845 ) ) ;
#2714 = CARTESIAN_POINT ( 'NONE',  ( 3.229347689422841228, -48.22934768942280925, -96.54999999890752349 ) ) ;
#2715 = CIRCLE ( 'NONE', #7630, 12.00000000000000000 ) ;
#2716 = ORIENTED_EDGE ( 'NONE', *, *, #4452, .T. ) ;
#2717 = DIRECTION ( 'NONE',  ( 1.000000000000000000, 0.000000000000000000, 0.000000000000000000 ) ) ;
#2718 = CARTESIAN_POINT ( 'NONE',  ( -23.98959235991431171, -46.50000000000000711, 6.010407640085604797 ) ) ;
#2719 = CARTESIAN_POINT ( 'NONE',  ( -39.39132668755255651, -42.69859572486944188, -1.433802505903950308 ) ) ;
#2720 = CARTESIAN_POINT ( 'NONE',  ( -20.62524821624488069, -39.20140427513058512, 1.538452329860250378 ) ) ;
#2721 = VERTEX_POINT ( 'NONE', #6109 ) ;
#2722 = VECTOR ( 'NONE', #4021, 1000.000000000000000 ) ;
#2723 = EDGE_LOOP ( 'NONE', ( #1341, #8385, #3252, #6587 ) ) ;
#2724 = CARTESIAN_POINT ( 'NONE',  ( -31.61762450863942320, -48.95140427513057091, 9.857197362228843573 ) ) ;
#2725 = AXIS2_PLACEMENT_3D ( 'NONE', #2465, #3174, #5147 ) ;
#2726 = CARTESIAN_POINT ( 'NONE',  ( -3.535533905932736864, -41.46446609406723383, -99.10000000000000853 ) ) ;
#2727 = CARTESIAN_POINT ( 'NONE',  ( -2.071067811865475061, -39.99999999999997158, -99.04999999781504982 ) ) ;
#2728 = CARTESIAN_POINT ( 'NONE',  ( 2.071067811865477282, -49.99999999999997158, -96.35000000000000853 ) ) ;
#2729 = CARTESIAN_POINT ( 'NONE',  ( -2.071067811865475505, -49.99999999999996447, -99.64999999999999147 ) ) ;
#2730 = ORIENTED_EDGE ( 'NONE', *, *, #893, .T. ) ;
#2731 = CARTESIAN_POINT ( 'NONE',  ( -33.81171626276147890, -33.09859572486943335, 7.597606577763319713 ) ) ;
#2732 = CARTESIAN_POINT ( 'NONE',  ( -20.61696076434619584, -31.20000000000000639, 1.486127417882100676 ) ) ;
#2733 = MECHANICAL_DESIGN_GEOMETRIC_PRESENTATION_REPRESENTATION (  '', ( #186 ), #3155 ) ;
#2734 = ORIENTED_EDGE ( 'NONE', *, *, #2094, .T. ) ;
#2735 = CARTESIAN_POINT ( 'NONE',  ( -2.796473189345805913E-16, -40.43301269999997061, -97.24999999890751212 ) ) ;
#2736 = ADVANCED_FACE ( 'NONE', ( #6724 ), #7475, .F. ) ;
#2737 = CIRCLE ( 'NONE', #751, 1.610000000000000098 ) ;
#2738 = CARTESIAN_POINT ( 'NONE',  ( 3.535533905932736420, -41.46446609406723383, -97.59999999781504698 ) ) ;
#2739 = CARTESIAN_POINT ( 'NONE',  ( -36.71751442127229836, -45.00000000000000711, -6.717514421272142044 ) ) ;
#2740 = CARTESIAN_POINT ( 'NONE',  ( 3.229347689422839895, -41.77065231057713390, -98.74999999890752633 ) ) ;
#2741 = APPLICATION_CONTEXT ( 'automotive_design' ) ;
#2742 = DIRECTION ( 'NONE',  ( 0.000000000000000000, 0.000000000000000000, -1.000000000000000000 ) ) ;
#2743 = CARTESIAN_POINT ( 'NONE',  ( -25.99212434019154472, -45.65140427513058086, 7.988596311142242890 ) ) ;
#2744 = VECTOR ( 'NONE', #2174, 1000.000000000000000 ) ;
#2745 = ADVANCED_FACE ( 'NONE', ( #6021 ), #7434, .F. ) ;
#2746 = CARTESIAN_POINT ( 'NONE',  ( -4.999999999999997335, -47.07106781186546129, -95.74300000002187971 ) ) ;
#2747 = CARTESIAN_POINT ( 'NONE',  ( -31.39812190974910422, -49.95000000000000995, 8.827394325379140483 ) ) ;
#2748 = EDGE_CURVE ( 'NONE', #7480, #2812, #5066, .T. ) ;
#2749 = CARTESIAN_POINT ( 'NONE',  ( 27.48332863331305731, -49.33273298888234848, 12.24717930254580267 ) ) ;
#2750 = DIRECTION ( 'NONE',  ( -0.000000000000000000, -0.000000000000000000, -1.000000000000000000 ) ) ;
#2751 = ITEM_DEFINED_TRANSFORMATION ( 'NONE', 'NONE', #4244,  #2554 ) ;
#2752 = VERTEX_POINT ( 'NONE', #1391 ) ;
#2753 = DIRECTION ( 'NONE',  ( -0.000000000000000000, -0.000000000000000000, 1.000000000000000000 ) ) ;
#2754 = CARTESIAN_POINT ( 'NONE',  ( -20.13408869516453947, -43.04999999999999005, -1.562606840307983136 ) ) ;
#2755 = CARTESIAN_POINT ( 'NONE',  ( -35.97294713907137975, -47.00140427513058938, -6.047868141099968398 ) ) ;
#2756 = DIRECTION ( 'NONE',  ( -1.000000000000000000, -0.000000000000000000, -0.000000000000000000 ) ) ;
#2757 = DIRECTION ( 'NONE',  ( 0.000000000000000000, 0.000000000000000000, 1.000000000000000000 ) ) ;
#2758 = CARTESIAN_POINT ( 'NONE',  ( -39.85719736222883824, -42.54859572486944330, 1.617624508639602388 ) ) ;
#2759 = FACE_OUTER_BOUND ( 'NONE', #3211, .T. ) ;
#2760 = FACE_OUTER_BOUND ( 'NONE', #1152, .T. ) ;
#2761 =( NAMED_UNIT ( * ) SI_UNIT ( $, .STERADIAN. ) SOLID_ANGLE_UNIT ( ) );
#2762 = ORIENTED_EDGE ( 'NONE', *, *, #7138, .F. ) ;
#2763 = DIRECTION ( 'NONE',  ( 0.000000000000000000, -1.000000000000000000, 0.000000000000000000 ) ) ;
#2764 = AXIS2_PLACEMENT_3D ( 'NONE', #7503, #2756, #3461 ) ;
#2765 = CARTESIAN_POINT ( 'NONE',  ( -31.38201786482021305, -31.29859572486943975, -8.387063443159975762 ) ) ;
#2766 = CARTESIAN_POINT ( 'NONE',  ( -20.14280263777121149, -41.04859572486944330, -1.617624508639600833 ) ) ;
#2767 = CARTESIAN_POINT ( 'NONE',  ( -34.36011273255026310, -46.10140427513058370, 8.440510857627391061 ) ) ;
#2768 = ORIENTED_EDGE ( 'NONE', *, *, #7411, .F. ) ;
#2769 = VERTEX_POINT ( 'NONE', #5395 ) ;
#2770 = CARTESIAN_POINT ( 'NONE',  ( -34.48522952044771017, -44.15140427513058086, -8.925456012876139766 ) ) ;
#2771 = EDGE_CURVE ( 'NONE', #2602, #3280, #4747, .T. ) ;
#2772 = ADVANCED_BREP_SHAPE_REPRESENTATION ( '', ( #2885, #2554 ), #1987 ) ;
#2773 = AXIS2_PLACEMENT_3D ( 'NONE', #7719, #8342, #4326 ) ;
#2774 = CARTESIAN_POINT ( 'NONE',  ( 42.00000000000000711, 48.00000000000002842, 20.34999999999992326 ) ) ;
#2775 = CARTESIAN_POINT ( 'NONE',  ( 3.229347689422841228, -48.22934768942280925, -95.94999999890751496 ) ) ;
#2776 = CARTESIAN_POINT ( 'NONE',  ( -49.99999999999997158, -59.99999999999997158, 30.00000000000000000 ) ) ;
#2777 = CARTESIAN_POINT ( 'NONE',  ( 42.00000000000000711, 48.00000000000002842, 21.99999999999992184 ) ) ;
#2778 = ORIENTED_EDGE ( 'NONE', *, *, #2371, .F. ) ;
#2779 = AXIS2_PLACEMENT_3D ( 'NONE', #8663, #1961, #5343 ) ;
#2780 = CARTESIAN_POINT ( 'NONE',  ( -26.18828373723858149, -34.59859572486944046, -7.597606577763319713 ) ) ;
#2781 = CARTESIAN_POINT ( 'NONE',  ( -28.51387258211773812, -37.80000000000000426, 9.383039235653802379 ) ) ;
#2782 = VECTOR ( 'NONE', #5290, 999.9999999999998863 ) ;
#2783 = ORIENTED_EDGE ( 'NONE', *, *, #4976, .F. ) ;
#2784 = CARTESIAN_POINT ( 'NONE',  ( -4.566987299999997418, -46.89170807884566017, -97.79999999890752349 ) ) ;
#2785 = CARTESIAN_POINT ( 'NONE',  ( -4.999999999999997335, -47.07106781186546129, -99.75000000000001421 ) ) ;
#2786 = CARTESIAN_POINT ( 'NONE',  ( -25.46513832392765408, -49.64999999999999147, 8.900167166472096270 ) ) ;
#2787 = VECTOR ( 'NONE', #5332, 1000.000000000000000 ) ;
#2788 = CARTESIAN_POINT ( 'NONE',  ( -3.229347689422840784, -41.77065231057713390, -96.94999999890751496 ) ) ;
#2789 = DIRECTION ( 'NONE',  ( 0.000000000000000000, 0.000000000000000000, 1.000000000000000000 ) ) ;
#2790 = CARTESIAN_POINT ( 'NONE',  ( -25.99212434019154472, -39.65140427513058086, 7.988596311142242890 ) ) ;
#2791 = CIRCLE ( 'NONE', #3909, 1.000000000000000888 ) ;
#2792 = CARTESIAN_POINT ( 'NONE',  ( -2.071067811865475505, -49.99999999999996447, -95.64300000002185698 ) ) ;
#2793 = CARTESIAN_POINT ( 'NONE',  ( -21.60464910494133406, -43.20000000000000995, 1.329692952841886155 ) ) ;
#2794 = SHAPE_DEFINITION_REPRESENTATION ( #8394, #4396 ) ;
#2795 = ORIENTED_EDGE ( 'NONE', *, *, #2611, .T. ) ;
#2796 = CARTESIAN_POINT ( 'NONE',  ( -31.56260684030781505, -46.94999999999998863, 9.865911304835510265 ) ) ;
#2797 = CARTESIAN_POINT ( 'NONE',  ( -37.59760657776328685, -46.40140427513058086, 3.811716262761598362 ) ) ;
#2798 = CARTESIAN_POINT ( 'NONE',  ( 30.00000000000000000, -39.99999999999998579, 12.49999999999996625 ) ) ;
#2799 = DIRECTION ( 'NONE',  ( -0.000000000000000000, -0.000000000000000000, 1.000000000000000000 ) ) ;
#2800 = CARTESIAN_POINT ( 'NONE',  ( -20.14280263777121149, -47.04859572486944330, -1.617624508639600833 ) ) ;
#2801 = DIRECTION ( 'NONE',  ( 0.5150380749100560429, 1.049727191138617340E-16, 0.8571673007021112234 ) ) ;
#2802 = CARTESIAN_POINT ( 'NONE',  ( -25.46513832392766119, -34.64999999999999858, 8.900167166472096270 ) ) ;
#2803 =( NAMED_UNIT ( * ) SI_UNIT ( $, .STERADIAN. ) SOLID_ANGLE_UNIT ( ) );
#2804 = ORIENTED_EDGE ( 'NONE', *, *, #8524, .T. ) ;
#2805 = CARTESIAN_POINT ( 'NONE',  ( 5.000000000000000000, -47.07106781186545419, -98.65000000000000568 ) ) ;
#2806 = ORIENTED_EDGE ( 'NONE', *, *, #4721, .T. ) ;
#2807 = CARTESIAN_POINT ( 'NONE',  ( -28.65689575858256077, -34.44859572486944188, -8.836108267985801845 ) ) ;
#2808 = CARTESIAN_POINT ( 'NONE',  ( -28.49241082802385350, -43.44859572486944188, -9.874625247442173404 ) ) ;
#2809 = CARTESIAN_POINT ( 'NONE',  ( -21.51138689804841420, -41.90140427513058086, -4.265706762501151772 ) ) ;
#2810 = MANIFOLD_SOLID_BREP ( 'Mirror1', #679 ) ;
#2811 = ORIENTED_EDGE ( 'NONE', *, *, #8254, .T. ) ;
#2812 = VERTEX_POINT ( 'NONE', #4791 ) ;
#2813 = CARTESIAN_POINT ( 'NONE',  ( 1.891708078845685481, -49.56698729999997255, -95.79999999890752349 ) ) ;
#2814 = FACE_OUTER_BOUND ( 'NONE', #6733, .T. ) ;
#2815 = CARTESIAN_POINT ( 'NONE',  ( -7.499999999999999112, -44.99999999999997158, -105.0000000000000142 ) ) ;
#2816 = CARTESIAN_POINT ( 'NONE',  ( -4.566987299999998307, -44.99999999999997158, -96.24999999890751212 ) ) ;
#2817 = CARTESIAN_POINT ( 'NONE',  ( -36.36396103067902175, -30.00000000000000711, -6.363961030678874309 ) ) ;
#2818 = CARTESIAN_POINT ( 'NONE',  ( -4.999999999999997335, -47.07106781186546129, -96.44999999781504130 ) ) ;
#2819 = ORIENTED_EDGE ( 'NONE', *, *, #4417, .F. ) ;
#2820 = CARTESIAN_POINT ( 'NONE',  ( -31.34310424141748896, -32.94859572486944188, 8.836108267985801845 ) ) ;
#2821 = CARTESIAN_POINT ( 'NONE',  ( -20.61696076434619584, -34.20000000000000995, 1.486127417882100676 ) ) ;
#2822 = ORIENTED_EDGE ( 'NONE', *, *, #8511, .F. ) ;
#2823 = CARTESIAN_POINT ( 'NONE',  ( -21.09983283352784156, -46.34999999999998721, 4.534861676072186043 ) ) ;
#2824 = AXIS2_PLACEMENT_3D ( 'NONE', #8000, #2712, #8617 ) ;
#2825 = CARTESIAN_POINT ( 'NONE',  ( 1.891708078845682595, -40.43301269999998482, -97.29999999890752349 ) ) ;
#2826 = CARTESIAN_POINT ( 'NONE',  ( 5.000000000000000000, -47.07106781186545419, -100.1499999978150441 ) ) ;
#2827 = CARTESIAN_POINT ( 'NONE',  ( -28.51387258211773812, -49.80000000000001137, 9.383039235653802379 ) ) ;
#2828 = CARTESIAN_POINT ( 'NONE',  ( -1.891708078845683039, -40.43301269999998482, -97.79999999890752349 ) ) ;
#2829 = CARTESIAN_POINT ( 'NONE',  ( -35.97294713907137975, -47.00140427513058938, -6.047868141099968398 ) ) ;
#2830 = AXIS2_PLACEMENT_3D ( 'NONE', #3421, #3331, #2143 ) ;
#2831 = CARTESIAN_POINT ( 'NONE',  ( 0.9662756667218486140, -39.99999999999997158, -100.0163279582177722 ) ) ;
#2832 = UNCERTAINTY_MEASURE_WITH_UNIT (LENGTH_MEASURE( 1.000000000000000082E-05 ), #3818, 'distance_accuracy_value', 'NONE');
#2833 = CARTESIAN_POINT ( 'NONE',  ( -2.796473189345805913E-16, -40.43301269999997061, -96.24999999890752633 ) ) ;
#2834 = CARTESIAN_POINT ( 'NONE',  ( -37.57355545560112375, -41.40000000000000568, 3.858919247786223305 ) ) ;
#2835 = CARTESIAN_POINT ( 'NONE',  ( -26.64110105645932336, 8.000000000000000000, 125.0000000000000000 ) ) ;
#2836 = APPLICATION_PROTOCOL_DEFINITION ( 'draft international standard', 'automotive_design', 1998, #7853 ) ;
#2837 = PRESENTATION_LAYER_ASSIGNMENT (  '', '', ( #5499 ) ) ;
#2838 = ORIENTED_EDGE ( 'NONE', *, *, #1692, .F. ) ;
#2839 = CYLINDRICAL_SURFACE ( 'NONE', #1935, 11.99999999999983302 ) ;
#2840 = DIRECTION ( 'NONE',  ( -1.000000000000000000, -0.000000000000000000, -0.000000000000000000 ) ) ;
#2841 = CARTESIAN_POINT ( 'NONE',  ( -26.14108075221394856, -36.60000000000000853, -7.573555455601170827 ) ) ;
#2842 = CARTESIAN_POINT ( 'NONE',  ( 28.37719198635490869, -40.25948930238541124, 12.39794155511764373 ) ) ;
#2843 = DIRECTION ( 'NONE',  ( 0.000000000000000000, 0.000000000000000000, -1.000000000000000000 ) ) ;
#2844 = CARTESIAN_POINT ( 'NONE',  ( -38.92545601287626056, -48.84859572486942625, -4.485229520447501450 ) ) ;
#2845 = ADVANCED_FACE ( 'NONE', ( #2061 ), #4269, .F. ) ;
#2846 = CARTESIAN_POINT ( 'NONE',  ( 2.000000000000000000, -0.8865213383406692627, 1.535500000000001641 ) ) ;
#2847 = DIRECTION ( 'NONE',  ( -0.000000000000000000, -0.000000000000000000, 1.000000000000000000 ) ) ;
#2848 = VERTEX_POINT ( 'NONE', #2017 ) ;
#2849 = DIRECTION ( 'NONE',  ( -1.000000000000000000, -0.000000000000000000, -0.000000000000000000 ) ) ;
#2850 = ORIENTED_EDGE ( 'NONE', *, *, #8100, .T. ) ;
#2851 = CARTESIAN_POINT ( 'NONE',  ( -37.98859631114233792, -36.84859572486944046, -4.007875659808334490 ) ) ;
#2852 = CARTESIAN_POINT ( 'NONE',  ( -39.85719736222883824, -36.54859572486943620, 1.617624508639602388 ) ) ;
#2853 = CARTESIAN_POINT ( 'NONE',  ( -38.87487832006816291, -43.85140427513058370, -4.584493831696867971 ) ) ;
#2854 = VECTOR ( 'NONE', #7379, 1000.000000000000000 ) ;
#2855 = ORIENTED_EDGE ( 'NONE', *, *, #926, .F. ) ;
#2856 = CARTESIAN_POINT ( 'NONE',  ( -1.891708078845683705, -49.56698729999997255, -97.49999999890752633 ) ) ;
#2857 = VECTOR ( 'NONE', #6022, 1000.000000000000000 ) ;
#2858 = VECTOR ( 'NONE', #5679, 1000.000000000000000 ) ;
#2859 = CARTESIAN_POINT ( 'NONE',  ( 42.00000000000000711, 60.00000000000002842, 23.64999999999992042 ) ) ;
#2860 = CARTESIAN_POINT ( 'NONE',  ( -2.796473189345805913E-16, -40.43301269999997061, -97.24999999890751212 ) ) ;
#2861 = DIRECTION ( 'NONE',  ( -0.000000000000000000, -0.000000000000000000, -1.000000000000000000 ) ) ;
#2862 = CYLINDRICAL_SURFACE ( 'NONE', #1208, 1.000000000000000888 ) ;
#2863 = EDGE_CURVE ( 'NONE', #207, #1713, #1165, .T. ) ;
#2864 = EDGE_LOOP ( 'NONE', ( #7292, #5058, #3473, #5473 ) ) ;
#2865 = CARTESIAN_POINT ( 'NONE',  ( -23.95213185889994989, -32.49859572486943904, 5.972947139071243861 ) ) ;
#2866 = CARTESIAN_POINT ( 'NONE',  ( -34.31290974752564438, -32.10000000000000142, 8.464561979789547053 ) ) ;
#2867 = AXIS2_PLACEMENT_3D ( 'NONE', #1051, #1005, #3743 ) ;
#2868 = CIRCLE ( 'NONE', #4543, 2.149999999999985256 ) ;
#2869 = EDGE_LOOP ( 'NONE', ( #1443, #6359, #3501, #6514 ) ) ;
#2870 = CARTESIAN_POINT ( 'NONE',  ( -36.71751442127229836, -48.00000000000000711, -6.717514421272142044 ) ) ;
#2871 = CARTESIAN_POINT ( 'NONE',  ( 2.000000000000000000, -1.773042676681341634, 2.493664996716660198E-15 ) ) ;
#2872 = CARTESIAN_POINT ( 'NONE',  ( -4.566987299999997418, -46.89170807884566017, -100.1999999989075292 ) ) ;
#2873 = CARTESIAN_POINT ( 'NONE',  ( -4.999999999999997335, -47.07106781186546129, -99.64999999781502993 ) ) ;
#2874 = DIRECTION ( 'NONE',  ( -0.000000000000000000, -1.000000000000000000, -0.000000000000000000 ) ) ;
#2875 = CARTESIAN_POINT ( 'NONE',  ( 8.389419568037416259E-16, -49.56698729999997255, -99.04999999890752349 ) ) ;
#2876 = VECTOR ( 'NONE', #6624, 1000.000000000000000 ) ;
#2877 = CARTESIAN_POINT ( 'NONE',  ( -34.00787565980851213, -44.15140427513058086, -7.988596311142238449 ) ) ;
#2878 = CARTESIAN_POINT ( 'NONE',  ( -3.061616997868382155E-16, -39.99999999999997158, -99.99300000002185129 ) ) ;
#2879 = DIRECTION ( 'NONE',  ( 1.000000000000000000, 0.000000000000000000, 0.000000000000000000 ) ) ;
#2880 = CARTESIAN_POINT ( 'NONE',  ( -21.17260567462091103, -49.05000000000000426, -1.398121909749241887 ) ) ;
#2881 = PRODUCT_DEFINITION ( 'UNKNOWN', '', #1724, #4236 ) ;
#2882 = CARTESIAN_POINT ( 'NONE',  ( 30.00000000000000000, -49.99999999999997158, 12.49999999999995914 ) ) ;
#2883 =( BOUNDED_CURVE ( )  B_SPLINE_CURVE ( 2, ( #7146, #393, #2359, #3101, #7679, #5037, #3757, #6971, #6442 ),
 .UNSPECIFIED., .F., .T. ) 
 B_SPLINE_CURVE_WITH_KNOTS ( ( 3, 2, 2, 2, 3 ),
 ( 0.5714285714285713969, 0.5892857142857143016, 0.6071428571428570953, 0.6250000000000000000, 0.6428571428571429047 ),
 .UNSPECIFIED. ) 
 CURVE ( )  GEOMETRIC_REPRESENTATION_ITEM ( )  RATIONAL_B_SPLINE_CURVE ( ( 1.000000000000000000, 0.9238795325112867385, 1.000000000000000000, 0.9238795325112867385, 1.000000000000000000, 0.9238795325112867385, 1.000000000000000000, 0.9238795325112867385, 1.000000000000000000 ) ) 
 REPRESENTATION_ITEM ( '' )  );
#2884 = AXIS2_PLACEMENT_3D ( 'NONE', #118, #2157, #4842 ) ;
#2885 = MANIFOLD_SOLID_BREP ( 'Fillet1', #527 ) ;
#2886 = PRODUCT_CONTEXT ( 'NONE', #5770, 'mechanical' ) ;
#2887 = CARTESIAN_POINT ( 'NONE',  ( 0.1999999999999987899, 4.041334437186265510E-16, -3.299999999999999822 ) ) ;
#2888 = CARTESIAN_POINT ( 'NONE',  ( -34.05750781543318340, -39.14999999999999147, -7.963307464738195840 ) ) ;
#2889 = CARTESIAN_POINT ( 'NONE',  ( -25.67300017005173274, -42.48926715326583547, 11.72748501658995579 ) ) ;
#2890 = FACE_OUTER_BOUND ( 'NONE', #4342, .T. ) ;
#2891 = CARTESIAN_POINT ( 'NONE',  ( -38.92545601287626056, -45.84859572486944046, -4.485229520447501450 ) ) ;
#2892 = DIRECTION ( 'NONE',  ( 0.000000000000000000, 0.000000000000000000, -1.000000000000000000 ) ) ;
#2893 = CARTESIAN_POINT ( 'NONE',  ( -39.86591130483550671, -35.55000000000000426, 1.562606840307984690 ) ) ;
#2894 = B_SPLINE_CURVE_WITH_KNOTS ( 'NONE', 1,
 ( #6451, #5663 ),
 .UNSPECIFIED., .F., .F.,
 ( 2, 2 ),
 ( 0.000000000000000000, 1.000000000000000000 ),
 .UNSPECIFIED. ) ;
#2895 = SHAPE_REPRESENTATION_RELATIONSHIP ( 'NONE' , 'NONE' ,  #6471, #3705 ) ;
#2896 = ORIENTED_EDGE ( 'NONE', *, *, #5886, .F. ) ;
#2897 = DIRECTION ( 'NONE',  ( 0.7071067811865556774, 0.000000000000000000, 0.7071067811865393571 ) ) ;
#2898 = EDGE_LOOP ( 'NONE', ( #7399, #7088, #4815, #7618 ) ) ;
#2899 = CARTESIAN_POINT ( 'NONE',  ( -34.10713997105786888, -40.14859572486943762, -7.938018618334151455 ) ) ;
#2900 = CARTESIAN_POINT ( 'NONE',  ( -23.28248557872775137, -31.50000000000000711, 6.717514421272141156 ) ) ;
#2901 = CARTESIAN_POINT ( 'NONE',  ( -35.97294713907137975, -29.00140427513058583, -6.047868141099968398 ) ) ;
#2902 = EDGE_CURVE ( 'NONE', #764, #4453, #6795, .T. ) ;
#2903 = ORIENTED_EDGE ( 'NONE', *, *, #7411, .T. ) ;
#2904 = CARTESIAN_POINT ( 'NONE',  ( 1.891708078845682595, -40.43301269999998482, -96.29999999890752349 ) ) ;
#2905 = DIRECTION ( 'NONE',  ( 0.000000000000000000, 0.000000000000000000, 1.000000000000000000 ) ) ;
#2906 = CARTESIAN_POINT ( 'NONE',  ( 4.566987300000000083, -46.89170807884565306, -99.09999999890752065 ) ) ;
#2907 = CARTESIAN_POINT ( 'NONE',  ( -25.25955351082667022, -46.62311395930105107, 11.56703930231305932 ) ) ;
#2908 = CIRCLE ( 'NONE', #3320, 1.649999999999998579 ) ;
#2909 = FACE_BOUND ( 'NONE', #766, .T. ) ;
#2910 = ORIENTED_EDGE ( 'NONE', *, *, #2638, .F. ) ;
#2911 = CARTESIAN_POINT ( 'NONE',  ( -38.40363834695740053, -39.69859572486944188, -1.277368040863739118 ) ) ;
#2912 = CARTESIAN_POINT ( 'NONE',  ( -25.68709025247441602, -45.60000000000000853, -8.464561979789547053 ) ) ;
#2913 = ORIENTED_EDGE ( 'NONE', *, *, #8104, .F. ) ;
#2914 = CARTESIAN_POINT ( 'NONE',  ( -34.31290974752564438, -47.10000000000000142, 8.464561979789547053 ) ) ;
#2915 = CYLINDRICAL_SURFACE ( 'NONE', #5169, 12.49999999999998046 ) ;
#2916 = FACE_OUTER_BOUND ( 'NONE', #4182, .T. ) ;
#2917 = DIRECTION ( 'NONE',  ( 0.000000000000000000, 0.000000000000000000, 1.000000000000000000 ) ) ;
#2918 = CARTESIAN_POINT ( 'NONE',  ( -30.00000000000002487, 0.000000000000000000, -44.00000000000000000 ) ) ;
#2919 = CARTESIAN_POINT ( 'NONE',  ( 8.389419568037416259E-16, -49.56698729999997255, -98.24999999890752633 ) ) ;
#2920 = EDGE_CURVE ( 'NONE', #6416, #8159, #7221, .T. ) ;
#2921 = ORIENTED_EDGE ( 'NONE', *, *, #2211, .T. ) ;
#2922 = CARTESIAN_POINT ( 'NONE',  ( -25.99212434019154472, -42.65140427513058086, 7.988596311142242890 ) ) ;
#2923 = CARTESIAN_POINT ( 'NONE',  ( 4.999999999999998224, -44.99999999999997158, -99.39300000002185698 ) ) ;
#2924 = CARTESIAN_POINT ( 'NONE',  ( -50.00000000000002842, 30.00000000000000000, 60.00000000000002842 ) ) ;
#2925 = CARTESIAN_POINT ( 'NONE',  ( -38.39535089505872634, -44.70000000000000284, -1.329692952841885267 ) ) ;
#2926 = DIRECTION ( 'NONE',  ( 1.000000000000000000, 0.000000000000000000, 0.000000000000000000 ) ) ;
#2927 = AXIS2_PLACEMENT_3D ( 'NONE', #116, #6283, #8195 ) ;
#2928 = AXIS2_PLACEMENT_3D ( 'NONE', #2582, #4073, #8657 ) ;
#2929 = CARTESIAN_POINT ( 'NONE',  ( -33.85891924778610473, -38.10000000000000853, 7.573555455601171715 ) ) ;
#2930 = EDGE_CURVE ( 'NONE', #5183, #1887, #2868, .T. ) ;
#2931 = CARTESIAN_POINT ( 'NONE',  ( -41.99999999999996447, 48.00000000000002842, -20.35000000000000142 ) ) ;
#2932 = CARTESIAN_POINT ( 'NONE',  ( -30.00000000000002842, 0.000000000000000000, -45.00000000000000000 ) ) ;
#2933 = CARTESIAN_POINT ( 'NONE',  ( -31.48612741788231517, -30.30000000000000782, -9.383039235653804155 ) ) ;
#2934 = CARTESIAN_POINT ( 'NONE',  ( -50.00000000000002842, 30.00000000000000000, 80.00000000000002842 ) ) ;
#2935 = CARTESIAN_POINT ( 'NONE',  ( -23.28248557872775137, -37.50000000000000711, 6.717514421272141156 ) ) ;
#2936 = AXIS2_PLACEMENT_3D ( 'NONE', #830, #2917, #6911 ) ;
#2937 = ORIENTED_EDGE ( 'NONE', *, *, #1822, .T. ) ;
#2938 = FACE_OUTER_BOUND ( 'NONE', #4171, .T. ) ;
#2939 = ORIENTED_EDGE ( 'NONE', *, *, #2461, .T. ) ;
#2940 = CARTESIAN_POINT ( 'NONE',  ( -23.95213185889994989, -41.49859572486943904, 5.972947139071243861 ) ) ;
#2941 = CARTESIAN_POINT ( 'NONE',  ( -38.44051085762733777, -45.39859572486944472, 4.360112732550414982 ) ) ;
#2942 = CARTESIAN_POINT ( 'NONE',  ( -36.68005392025794009, -50.00140427513058938, -6.754974922286504757 ) ) ;
#2943 = CARTESIAN_POINT ( 'NONE',  ( 4.566987299999998307, -43.10829192115428299, -95.59999999890754907 ) ) ;
#2944 = DIRECTION ( 'NONE',  ( -1.000000000000000000, -1.224646799147352961E-16, 0.000000000000000000 ) ) ;
#2945 = CARTESIAN_POINT ( 'NONE',  ( -30.00000000000002487, 0.000000000000000000, -29.65000000000000213 ) ) ;
#2946 = CARTESIAN_POINT ( 'NONE',  ( 1.891708078845685481, -49.56698729999997255, -98.39999999890753202 ) ) ;
#2947 = CARTESIAN_POINT ( 'NONE',  ( -34.35889894354067309, 8.000000000000000000, -24.00000000000000000 ) ) ;
#2948 = CARTESIAN_POINT ( 'NONE',  ( 9.184850993605145972E-16, -49.99999999999997158, -96.29999999781504982 ) ) ;
#2949 = CYLINDRICAL_SURFACE ( 'NONE', #3, 2.000000000000000888 ) ;
#2950 = EDGE_LOOP ( 'NONE', ( #6701, #824, #4740, #2164 ) ) ;
#2951 = EDGE_CURVE ( 'NONE', #1713, #207, #5673, .T. ) ;
#2952 = AXIS2_PLACEMENT_3D ( 'NONE', #3355, #5272, #6641 ) ;
#2953 = CARTESIAN_POINT ( 'NONE',  ( -36.04786814110010340, -36.99859572486943193, -5.972947139071243861 ) ) ;
#2954 = CARTESIAN_POINT ( 'NONE',  ( -31.56260684030781505, -40.95000000000000995, 9.865911304835510265 ) ) ;
#2955 = VERTEX_POINT ( 'NONE', #7648 ) ;
#2956 = CARTESIAN_POINT ( 'NONE',  ( -31.43380250590416125, -29.30140427513058299, -9.391326687552492558 ) ) ;
#2957 = PRESENTATION_STYLE_ASSIGNMENT (( #4802 ) ) ;
#2958 = SPHERICAL_SURFACE ( 'NONE', #5145, 1.000000000000000000 ) ;
#2959 = MANIFOLD_SOLID_BREP ( 'Hex', #4355 ) ;
#2960 = CARTESIAN_POINT ( 'NONE',  ( -3.535533905932735532, -48.53553390593270933, -98.79999999781504982 ) ) ;
#2961 = DIRECTION ( 'NONE',  ( 0.000000000000000000, 0.000000000000000000, 1.000000000000000000 ) ) ;
#2962 = CARTESIAN_POINT ( 'NONE',  ( -3.229347689422839451, -48.22934768942280925, -99.14999999890753202 ) ) ;
#2963 = EDGE_CURVE ( 'NONE', #4661, #7038, #2025, .T. ) ;
#2964 = VERTEX_POINT ( 'NONE', #5533 ) ;
#2965 = CARTESIAN_POINT ( 'NONE',  ( -33.85891924778610473, -32.10000000000000142, 7.573555455601171715 ) ) ;
#2966 = CARTESIAN_POINT ( 'NONE',  ( -4.999999999999998224, -42.92893218813448897, -98.24300000002185129 ) ) ;
#2967 = CARTESIAN_POINT ( 'NONE',  ( -33.35889894354067309, -7.999999999999996447, -23.99999999999999289 ) ) ;
#2968 = CARTESIAN_POINT ( 'NONE',  ( -4.999999999999998224, -44.99999999999997158, -96.49999999781503845 ) ) ;
#2969 = DIRECTION ( 'NONE',  ( -0.000000000000000000, 1.000000000000000000, -0.000000000000000000 ) ) ;
#2970 = EDGE_CURVE ( 'NONE', #7654, #7480, #7041, .T. ) ;
#2971 = CONTEXT_DEPENDENT_SHAPE_REPRESENTATION ( #5830, #6387 ) ;
#2972 = CARTESIAN_POINT ( 'NONE',  ( -38.39535089505872634, -41.70000000000000995, -1.329692952841885267 ) ) ;
#2973 = PRODUCT_DEFINITION_SHAPE ( 'NONE', 'NONE',  #5874 ) ;
#2974 = CARTESIAN_POINT ( 'NONE',  ( 4.566987299999998307, -43.10829192115428299, -95.79999999890752349 ) ) ;
#2975 = CARTESIAN_POINT ( 'NONE',  ( -45.00000000000003553, -44.99999999999997158, 0.000000000000000000 ) ) ;
#2976 = CARTESIAN_POINT ( 'NONE',  ( -39.86591130483550671, -35.55000000000001137, 1.562606840307984468 ) ) ;
#2977 = CARTESIAN_POINT ( 'NONE',  ( 4.200000000000001954, 0.000000000000000000, 2.000000000000000888 ) ) ;
#2978 = AXIS2_PLACEMENT_3D ( 'NONE', #3039, #6372, #5842 ) ;
#2979 = CARTESIAN_POINT ( 'NONE',  ( -34.31290974752564438, -44.10000000000000853, 8.464561979789547053 ) ) ;
#2980 = FILL_AREA_STYLE_COLOUR ( '', #3828 ) ;
#2981 = ORIENTED_EDGE ( 'NONE', *, *, #1, .T. ) ;
#2982 = CARTESIAN_POINT ( 'NONE',  ( 42.00000000000000711, 60.00000000000002842, 21.99999999999992184 ) ) ;
#2983 = ORIENTED_EDGE ( 'NONE', *, *, #893, .F. ) ;
#2984 = CARTESIAN_POINT ( 'NONE',  ( -31.34310424141748896, -38.94859572486943478, 8.836108267985801845 ) ) ;
#2985 = CARTESIAN_POINT ( 'NONE',  ( -36.75497492228666374, -48.99859572486944614, -6.680053920257780220 ) ) ;
#2986 = CARTESIAN_POINT ( 'NONE',  ( -31.45313957808072303, -30.95140427513058157, 8.818680382772479120 ) ) ;
#2987 =( GEOMETRIC_REPRESENTATION_CONTEXT ( 3 ) GLOBAL_UNCERTAINTY_ASSIGNED_CONTEXT ( ( #6434 ) ) GLOBAL_UNIT_ASSIGNED_CONTEXT ( ( #6932, #6316, #1111 ) ) REPRESENTATION_CONTEXT ( 'NONE', 'WORKASPACE' ) );
#2988 = CARTESIAN_POINT ( 'NONE',  ( 4.566987299999998307, -43.10829192115428299, -97.99999999890752633 ) ) ;
#2989 = CARTESIAN_POINT ( 'NONE',  ( -20.61696076434619584, -31.20000000000000639, 1.486127417882100676 ) ) ;
#2990 = CARTESIAN_POINT ( 'NONE',  ( 3.229347689422841228, -48.22934768942280925, -98.34999999890752065 ) ) ;
#2991 = CARTESIAN_POINT ( 'NONE',  ( -29.33468802289397104, -49.96635986460699286, 12.48644052906006685 ) ) ;
#2992 = CARTESIAN_POINT ( 'NONE',  ( 1.891708078845682595, -40.43301269999998482, -96.49999999890752633 ) ) ;
#2993 = LINE ( 'NONE', #5014, #1271 ) ;
#2994 = ORIENTED_EDGE ( 'NONE', *, *, #7917, .F. ) ;
#2995 = AXIS2_PLACEMENT_3D ( 'NONE', #5873, #3845, #5246 ) ;
#2996 = CARTESIAN_POINT ( 'NONE',  ( -22.01140368885771892, -44.34859572486944046, 4.007875659808335378 ) ) ;
#2997 = CARTESIAN_POINT ( 'NONE',  ( -21.53543802021056663, -39.90000000000000568, -4.312909747525783821 ) ) ;
#2998 = EDGE_CURVE ( 'NONE', #1128, #5614, #2153, .T. ) ;
#2999 = VECTOR ( 'NONE', #4748, 1000.000000000000000 ) ;
#3000 = ORIENTED_EDGE ( 'NONE', *, *, #3495, .T. ) ;
#3001 = CARTESIAN_POINT ( 'NONE',  ( -38.90016716647221529, -44.85000000000001563, -4.534861676072185155 ) ) ;
#3002 = FACE_OUTER_BOUND ( 'NONE', #3862, .T. ) ;
#3003 = CARTESIAN_POINT ( 'NONE',  ( 3.229347689422839895, -41.77065231057713390, -99.74999999890751212 ) ) ;
#3004 = CARTESIAN_POINT ( 'NONE',  ( 4.999999999999998224, -42.92893218813448897, -99.24999999781506688 ) ) ;
#3005 = CARTESIAN_POINT ( 'NONE',  ( -4.999999999999998224, -44.99999999999997158, -95.00000000000000000 ) ) ;
#3006 = CARTESIAN_POINT ( 'NONE',  ( -4.999999999999998224, -44.99999999999997158, -95.79999999999999716 ) ) ;
#3007 = ORIENTED_EDGE ( 'NONE', *, *, #7941, .F. ) ;
#3008 = CARTESIAN_POINT ( 'NONE',  ( -36.01040764008574513, -33.00000000000000711, -6.010407640085605685 ) ) ;
#3009 = EDGE_CURVE ( 'NONE', #5109, #1663, #1172, .T. ) ;
#3010 = CARTESIAN_POINT ( 'NONE',  ( 2.071067811865474173, -39.99999999999997158, -95.25000000000000000 ) ) ;
#3011 = CARTESIAN_POINT ( 'NONE',  ( 34.00000000000000000, 1.610000000000000098, 0.000000000000000000 ) ) ;
#3012 = CIRCLE ( 'NONE', #2725, 12.00000000000000000 ) ;
#3013 = CARTESIAN_POINT ( 'NONE',  ( 3.535533905932736420, -41.46446609406723383, -96.79999999781504982 ) ) ;
#3014 = DIRECTION ( 'NONE',  ( 1.000000000000000000, -0.000000000000000000, -0.000000000000000000 ) ) ;
#3015 = ITEM_DEFINED_TRANSFORMATION ( 'NONE', 'NONE', #5508,  #2554 ) ;
#3016 = ADVANCED_FACE ( 'NONE', ( #2814 ), #6195, .T. ) ;
#3017 = CARTESIAN_POINT ( 'NONE',  ( -39.84999999999998010, 22.00000000000000000, 80.00000000000002842 ) ) ;
#3018 = CARTESIAN_POINT ( 'NONE',  ( -34.05750781543318340, -36.15000000000001279, -7.963307464738195840 ) ) ;
#3019 = EDGE_CURVE ( 'NONE', #58, #3140, #4277, .T. ) ;
#3020 = EDGE_CURVE ( 'NONE', #2150, #3379, #4866, .T. ) ;
#3021 = CARTESIAN_POINT ( 'NONE',  ( 3.229347689422839895, -41.77065231057713390, -95.74999999890751212 ) ) ;
#3022 = CARTESIAN_POINT ( 'NONE',  ( -26.14108075221394856, -30.60000000000000142, -7.573555455601170827 ) ) ;
#3023 = CARTESIAN_POINT ( 'NONE',  ( -28.51387258211773812, -34.80000000000000426, 9.383039235653802379 ) ) ;
#3024 = AXIS2_PLACEMENT_3D ( 'NONE', #1039, #4393, #8530 ) ;
#3025 = LINE ( 'NONE', #1740, #1699 ) ;
#3026 = CARTESIAN_POINT ( 'NONE',  ( -38.90016716647221529, -44.85000000000000853, -4.534861676072185155 ) ) ;
#3027 = SURFACE_STYLE_USAGE ( .BOTH. , #7067 ) ;
#3028 = ORIENTED_EDGE ( 'NONE', *, *, #1265, .T. ) ;
#3029 = ORIENTED_EDGE ( 'NONE', *, *, #8716, .T. ) ;
#3030 = CARTESIAN_POINT ( 'NONE',  ( -22.45049566656107842, -34.89859572486943762, -3.906122232810846917 ) ) ;
#3031 = CARTESIAN_POINT ( 'NONE',  ( -36.75497492228666374, -51.99859572486943193, -6.680053920257780220 ) ) ;
#3032 = CARTESIAN_POINT ( 'NONE',  ( -22.40239342223677355, -32.90140427513058086, -3.811716262761597473 ) ) ;
#3033 = CARTESIAN_POINT ( 'NONE',  ( -3.229347689422839451, -48.22934768942280925, -98.34999999890753486 ) ) ;
#3034 = CARTESIAN_POINT ( 'NONE',  ( 2.000000000000000000, -0.8865213383406692627, 1.535500000000001641 ) ) ;
#3035 = CARTESIAN_POINT ( 'NONE',  ( -36.71751442127229836, -36.00000000000000711, -6.717514421272142044 ) ) ;
#3036 = CARTESIAN_POINT ( 'NONE',  ( -2.796473189345805913E-16, -40.43301269999997061, -100.4499999989075292 ) ) ;
#3037 = LINE ( 'NONE', #370, #7228 ) ;
#3038 = CARTESIAN_POINT ( 'NONE',  ( -3.229347689422840784, -41.77065231057713390, -95.54999999890752349 ) ) ;
#3039 = CARTESIAN_POINT ( 'NONE',  ( 0.000000000000000000, -44.99999999999997158, -95.00000000000000000 ) ) ;
#3040 = ORIENTED_EDGE ( 'NONE', *, *, #6027, .T. ) ;
#3041 = CARTESIAN_POINT ( 'NONE',  ( -28.61798213517984024, -38.79859572486943620, 8.387063443159973986 ) ) ;
#3042 = CARTESIAN_POINT ( 'NONE',  ( -37.06321265474346660, -47.25000000000000711, 7.063212654743582952 ) ) ;
#3043 = EDGE_CURVE ( 'NONE', #6389, #899, #3579, .T. ) ;
#3044 = ORIENTED_EDGE ( 'NONE', *, *, #4327, .F. ) ;
#3045 = CARTESIAN_POINT ( 'NONE',  ( -28.56619749409589204, -39.80140427513057944, 9.391326687552490782 ) ) ;
#3046 = CARTESIAN_POINT ( 'NONE',  ( 3.535533905932736420, -41.46446609406723383, -96.79999999781504982 ) ) ;
#3047 = DIRECTION ( 'NONE',  ( 0.000000000000000000, 0.000000000000000000, -1.000000000000000000 ) ) ;
#3048 = MANIFOLD_SOLID_BREP ( 'Sweep1', #7016 ) ;
#3049 = CARTESIAN_POINT ( 'NONE',  ( 29.99999999999997158, 1.102182119232617753E-14, 80.00000000000002842 ) ) ;
#3050 = CYLINDRICAL_SURFACE ( 'NONE', #7494, 12.00000000000000000 ) ;
#3051 = CARTESIAN_POINT ( 'NONE',  ( -3.535533905932735532, -48.53553390593270933, -97.29999999999999716 ) ) ;
#3052 = ORIENTED_EDGE ( 'NONE', *, *, #6376, .T. ) ;
#3053 = CARTESIAN_POINT ( 'NONE',  ( -34.05750781543318340, -36.15000000000001279, -7.963307464738195840 ) ) ;
#3054 = ORIENTED_EDGE ( 'NONE', *, *, #8104, .T. ) ;
#3055 = CARTESIAN_POINT ( 'NONE',  ( 4.999999999999998224, -42.92893218813448897, -97.75000000000001421 ) ) ;
#3056 = CARTESIAN_POINT ( 'NONE',  ( 2.071067811865477282, -49.99999999999996447, -97.04999999781504982 ) ) ;
#3057 = DIRECTION ( 'NONE',  ( -0.000000000000000000, 1.000000000000000000, -0.000000000000000000 ) ) ;
#3058 = CIRCLE ( 'NONE', #1923, 0.2000000000000000944 ) ;
#3059 = DIRECTION ( 'NONE',  ( -0.000000000000000000, -0.000000000000000000, 1.000000000000000000 ) ) ;
#3060 = CARTESIAN_POINT ( 'NONE',  ( -37.57355545560112375, -44.40000000000000568, 3.858919247786223305 ) ) ;
#3061 = AXIS2_PLACEMENT_3D ( 'NONE', #6113, #4264, #6816 ) ;
#3062 = FACE_BOUND ( 'NONE', #7511, .T. ) ;
#3063 = CARTESIAN_POINT ( 'NONE',  ( -30.00000000000000000, 0.000000000000000000, 80.00000000000002842 ) ) ;
#3064 = DIRECTION ( 'NONE',  ( -0.000000000000000000, -0.000000000000000000, 1.000000000000000000 ) ) ;
#3065 = CARTESIAN_POINT ( 'NONE',  ( -36.71751442127229836, -39.00000000000000711, -6.717514421272142044 ) ) ;
#3066 = DIRECTION ( 'NONE',  ( -0.000000000000000000, -0.000000000000000000, -1.000000000000000000 ) ) ;
#3067 = CARTESIAN_POINT ( 'NONE',  ( -34.53486167607238855, -36.15000000000000568, -8.900167166472096270 ) ) ;
#3068 = CIRCLE ( 'NONE', #7984, 1.649999999999998579 ) ;
#3069 = VERTEX_POINT ( 'NONE', #5180 ) ;
#3070 = CARTESIAN_POINT ( 'NONE',  ( -25.89286002894218086, -44.64859572486944472, 7.938018618334153231 ) ) ;
#3071 = CARTESIAN_POINT ( 'NONE',  ( -31.50758917197619979, -44.94859572486942767, 9.874625247442176956 ) ) ;
#3072 = CARTESIAN_POINT ( 'NONE',  ( -39.37475178375516549, -49.70140427513058512, -1.538452329860249712 ) ) ;
#3073 = CIRCLE ( 'NONE', #5737, 1.000000000000000888 ) ;
#3074 = CARTESIAN_POINT ( 'NONE',  ( -2.796473189345805913E-16, -40.43301269999997061, -99.44999999890752918 ) ) ;
#3075 = CARTESIAN_POINT ( 'NONE',  ( 32.51929462645154700, -40.66893875716690587, 12.24660140962717136 ) ) ;
#3076 = CARTESIAN_POINT ( 'NONE',  ( -20.13408869516453947, -37.05000000000001137, -1.562606840307983136 ) ) ;
#3077 = CARTESIAN_POINT ( 'NONE',  ( -30.00000000000002487, 0.000000000000000000, -29.65000000000000213 ) ) ;
#3078 = DIRECTION ( 'NONE',  ( -1.000000000000000000, -0.000000000000000000, -0.000000000000000000 ) ) ;
#3079 = CARTESIAN_POINT ( 'NONE',  ( -2.796473189345805913E-16, -40.43301269999997061, -97.24999999890751212 ) ) ;
#3080 = DIRECTION ( 'NONE',  ( -0.5000000000000061062, 0.000000000000000000, 0.8660254037844351549 ) ) ;
#3081 = ORIENTED_EDGE ( 'NONE', *, *, #5478, .F. ) ;
#3082 = CARTESIAN_POINT ( 'NONE',  ( -38.81868038277247734, -45.54859572486944330, 1.453139578080855365 ) ) ;
#3083 = CARTESIAN_POINT ( 'NONE',  ( -25.68709025247441602, -48.60000000000000142, -8.464561979789547053 ) ) ;
#3084 = ORIENTED_EDGE ( 'NONE', *, *, #995, .F. ) ;
#3085 = CARTESIAN_POINT ( 'NONE',  ( -23.31994607974211675, -33.50140427513058228, 6.754974922286503869 ) ) ;
#3086 = DIRECTION ( 'NONE',  ( -0.000000000000000000, -0.000000000000000000, 1.000000000000000000 ) ) ;
#3087 = CARTESIAN_POINT ( 'NONE',  ( 4.200000000000001954, 0.000000000000000000, -2.200000000000001066 ) ) ;
#3088 = DIRECTION ( 'NONE',  ( 1.049727191138618079E-16, 0.5150380749100549327, -0.8571673007021118895 ) ) ;
#3089 = DIRECTION ( 'NONE',  ( -1.000000000000000000, -0.000000000000000000, -0.000000000000000000 ) ) ;
#3090 = CARTESIAN_POINT ( 'NONE',  ( -3.061616997868382155E-16, -39.99999999999997158, -96.00000000000000000 ) ) ;
#3091 = ORIENTED_EDGE ( 'NONE', *, *, #6940, .F. ) ;
#3092 = CARTESIAN_POINT ( 'NONE',  ( -35.97294713907137975, -50.00140427513058938, -6.047868141099968398 ) ) ;
#3093 = EDGE_LOOP ( 'NONE', ( #2258, #2250, #3678, #323, #5773 ) ) ;
#3094 = CARTESIAN_POINT ( 'NONE',  ( -2.071067811865475505, -49.99999999999996447, -98.85000000000002274 ) ) ;
#3095 = DIRECTION ( 'NONE',  ( -1.000000000000000000, -0.000000000000000000, 0.000000000000000000 ) ) ;
#3096 = DIRECTION ( 'NONE',  ( -1.000000000000000000, 0.000000000000000000, 0.000000000000000000 ) ) ;
#3097 = ITEM_DEFINED_TRANSFORMATION ( 'NONE', 'NONE', #5650,  #2554 ) ;
#3098 = CARTESIAN_POINT ( 'NONE',  ( -40.00000000000002842, 1.224646799147353256E-15, -45.00000000000000000 ) ) ;
#3099 = CARTESIAN_POINT ( 'NONE',  ( 33.61000000000001364, 0.000000000000000000, 0.000000000000000000 ) ) ;
#3100 = AXIS2_PLACEMENT_3D ( 'NONE', #3419, #1596, #6270 ) ;
#3101 = CARTESIAN_POINT ( 'NONE',  ( -2.071067811865475061, -39.99999999999997158, -98.35000000000000853 ) ) ;
#3102 = CARTESIAN_POINT ( 'NONE',  ( 0.000000000000000000, 0.8865213383406717051, 1.535499999999999199 ) ) ;
#3103 = CARTESIAN_POINT ( 'NONE',  ( -30.00000000000000000, -49.99999999999997158, 12.49999999999997335 ) ) ;
#3104 = CARTESIAN_POINT ( 'NONE',  ( -20.61696076434619584, -43.20000000000000995, 1.486127417882100676 ) ) ;
#3105 = EDGE_CURVE ( 'NONE', #6677, #5152, #1504, .T. ) ;
#3106 =( NAMED_UNIT ( * ) PLANE_ANGLE_UNIT ( ) SI_UNIT ( $, .RADIAN. ) );
#3107 = EDGE_LOOP ( 'NONE', ( #537, #4130, #8427, #2850 ) ) ;
#3108 = CARTESIAN_POINT ( 'NONE',  ( -31.34310424141748896, -44.94859572486942767, 8.836108267985801845 ) ) ;
#3109 = CARTESIAN_POINT ( 'NONE',  ( -21.09983283352784156, -34.35000000000000853, 4.534861676072186043 ) ) ;
#3110 = CARTESIAN_POINT ( 'NONE',  ( -26.09387776718931917, -35.60140427513057659, -7.549504333439021941 ) ) ;
#3111 = AXIS2_PLACEMENT_3D ( 'NONE', #4780, #6186, #2231 ) ;
#3112 =( BOUNDED_CURVE ( )  B_SPLINE_CURVE ( 2, ( #765, #2805, #6755, #811, #107, #1471, #4165, #5301, #8004 ),
 .UNSPECIFIED., .F., .F. ) 
 B_SPLINE_CURVE_WITH_KNOTS ( ( 3, 2, 2, 2, 3 ),
 ( 0.6428571428571429047, 0.6607142857142856984, 0.6785714285714286031, 0.6964285714285713969, 0.7142857142857143016 ),
 .UNSPECIFIED. ) 
 CURVE ( )  GEOMETRIC_REPRESENTATION_ITEM ( )  RATIONAL_B_SPLINE_CURVE ( ( 1.000000000000000000, 0.9238795325112867385, 1.000000000000000000, 0.9238795325112867385, 1.000000000000000000, 0.9238795325112867385, 1.000000000000000000, 0.9238795325112867385, 1.000000000000000000 ) ) 
 REPRESENTATION_ITEM ( '' )  );
#3113 = EDGE_CURVE ( 'NONE', #196, #7832, #7874, .T. ) ;
#3114 = CARTESIAN_POINT ( 'NONE',  ( -2.071067811865475061, -39.99999999999997158, -95.95000000000001705 ) ) ;
#3115 = CIRCLE ( 'NONE', #7328, 1.000000000000000888 ) ;
#3116 = DIRECTION ( 'NONE',  ( -1.000000000000000000, 0.000000000000000000, 0.000000000000000000 ) ) ;
#3117 = CARTESIAN_POINT ( 'NONE',  ( -34.31290974752564438, -35.10000000000000853, 8.464561979789547053 ) ) ;
#3118 = CARTESIAN_POINT ( 'NONE',  ( 4.566987299999998307, -44.99999999999997158, -99.84999999890752065 ) ) ;
#3119 = LINE ( 'NONE', #7119, #5124 ) ;
#3120 = CARTESIAN_POINT ( 'NONE',  ( 8.389419568037416259E-16, -49.56698729999997255, -97.64999999890751781 ) ) ;
#3121 = VERTEX_POINT ( 'NONE', #7248 ) ;
#3122 = CARTESIAN_POINT ( 'NONE',  ( -49.99999999999997158, -59.99999999999997158, 30.00000000000000000 ) ) ;
#3123 = CARTESIAN_POINT ( 'NONE',  ( -25.41550616830297571, -32.64859572486943762, 8.874878320068054549 ) ) ;
#3124 = CARTESIAN_POINT ( 'NONE',  ( -23.31994607974211675, -30.50140427513058583, 6.754974922286503869 ) ) ;
#3125 = PRESENTATION_LAYER_ASSIGNMENT (  '', '', ( #2556 ) ) ;
#3126 = EDGE_CURVE ( 'NONE', #8149, #8159, #451, .T. ) ;
#3127 = VERTEX_POINT ( 'NONE', #8535 ) ;
#3128 = CARTESIAN_POINT ( 'NONE',  ( -34.36011273255026310, -40.10140427513057659, 8.440510857627391061 ) ) ;
#3129 = CARTESIAN_POINT ( 'NONE',  ( 2.071067811865474173, -39.99999999999997158, -96.74999999781503845 ) ) ;
#3130 = DIRECTION ( 'NONE',  ( 0.000000000000000000, 0.000000000000000000, 1.000000000000000000 ) ) ;
#3131 = EDGE_CURVE ( 'NONE', #1305, #2514, #6801, .T. ) ;
#3132 = CARTESIAN_POINT ( 'NONE',  ( 5.000000000000004441, -47.07106781186543998, -97.04999999999999716 ) ) ;
#3133 = AXIS2_PLACEMENT_3D ( 'NONE', #660, #476, #7991 ) ;
#3134 = CARTESIAN_POINT ( 'NONE',  ( -30.00000000000002487, 0.000000000000000000, -28.65000000000000213 ) ) ;
#3135 = CARTESIAN_POINT ( 'NONE',  ( 5.000000000000000000, -47.07106781186545419, -95.45000000000000284 ) ) ;
#3136 = ORIENTED_EDGE ( 'NONE', *, *, #6699, .T. ) ;
#3137 = CARTESIAN_POINT ( 'NONE',  ( -23.68028341417693738, -33.75000000000001421, -6.319716585823198507 ) ) ;
#3138 = EDGE_CURVE ( 'NONE', #2506, #6156, #2446, .T. ) ;
#3139 = CARTESIAN_POINT ( 'NONE',  ( -25.99212434019154472, -30.65140427513057730, 7.988596311142242890 ) ) ;
#3140 = VERTEX_POINT ( 'NONE', #1796 ) ;
#3141 = CARTESIAN_POINT ( 'NONE',  ( 2.071067811865474173, -39.99999999999997158, -99.25000000000000000 ) ) ;
#3142 = VECTOR ( 'NONE', #5736, 1000.000000000000000 ) ;
#3143 = CARTESIAN_POINT ( 'NONE',  ( 3.991994717416610161, -48.02431555730691315, -100.0008018208966831 ) ) ;
#3144 = CARTESIAN_POINT ( 'NONE',  ( -50.00000000000002842, 30.00000000000000000, 80.00000000000002842 ) ) ;
#3145 = CYLINDRICAL_SURFACE ( 'NONE', #1289, 4.999999999999998224 ) ;
#3146 = ADVANCED_FACE ( 'NONE', ( #3249 ), #3297, .T. ) ;
#3147 = AXIS2_PLACEMENT_3D ( 'NONE', #5871, #5914, #3976 ) ;
#3148 = EDGE_CURVE ( 'NONE', #876, #4620, #4479, .T. ) ;
#3149 =( GEOMETRIC_REPRESENTATION_CONTEXT ( 3 ) GLOBAL_UNCERTAINTY_ASSIGNED_CONTEXT ( ( #90 ) ) GLOBAL_UNIT_ASSIGNED_CONTEXT ( ( #727, #2639, #3344 ) ) REPRESENTATION_CONTEXT ( 'NONE', 'WORKASPACE' ) );
#3150 = DIRECTION ( 'NONE',  ( -1.000000000000000000, -0.000000000000000000, -0.000000000000000000 ) ) ;
#3151 = DIRECTION ( 'NONE',  ( -1.000000000000000000, -0.000000000000000000, -0.000000000000000000 ) ) ;
#3152 = CARTESIAN_POINT ( 'NONE',  ( 50.00000000000002842, 30.00000000000000000, 60.00000000000002842 ) ) ;
#3153 = CARTESIAN_POINT ( 'NONE',  ( -39.86591130483550671, -47.55000000000000426, 1.562606840307984690 ) ) ;
#3154 =( NAMED_UNIT ( * ) PLANE_ANGLE_UNIT ( ) SI_UNIT ( $, .RADIAN. ) );
#3155 =( GEOMETRIC_REPRESENTATION_CONTEXT ( 3 ) GLOBAL_UNCERTAINTY_ASSIGNED_CONTEXT ( ( #4471 ) ) GLOBAL_UNIT_ASSIGNED_CONTEXT ( ( #7559, #1658, #287 ) ) REPRESENTATION_CONTEXT ( 'NONE', 'WORKASPACE' ) );
#3156 = ORIENTED_EDGE ( 'NONE', *, *, #4757, .T. ) ;
#3157 = CARTESIAN_POINT ( 'NONE',  ( -22.45049566656107842, -49.89859572486943762, -3.906122232810846917 ) ) ;
#3158 = CARTESIAN_POINT ( 'NONE',  ( -20.13408869516453947, -34.04999999999998295, -1.562606840307983136 ) ) ;
#3159 = CARTESIAN_POINT ( 'NONE',  ( -25.99212434019154472, -36.65140427513058086, 7.988596311142242890 ) ) ;
#3160 = CIRCLE ( 'NONE', #2884, 1.000000000000000888 ) ;
#3161 = CARTESIAN_POINT ( 'NONE',  ( -5.000000000000000888, -42.92893218813449607, -95.85000000000000853 ) ) ;
#3162 = CARTESIAN_POINT ( 'NONE',  ( 30.65872425187075123, -40.04081516742414948, 12.48372095990569797 ) ) ;
#3163 = CARTESIAN_POINT ( 'NONE',  ( -23.24502507771338600, -35.49859572486943193, 6.680053920257780220 ) ) ;
#3164 = CARTESIAN_POINT ( 'NONE',  ( -22.93678734525658314, -33.75000000000001421, -7.063212654743582952 ) ) ;
#3165 = DIRECTION ( 'NONE',  ( 0.000000000000000000, 0.000000000000000000, 1.000000000000000000 ) ) ;
#3166 = DIRECTION ( 'NONE',  ( 0.000000000000000000, 0.000000000000000000, -1.000000000000000000 ) ) ;
#3167 = CARTESIAN_POINT ( 'NONE',  ( 8.389419568037416259E-16, -49.56698729999997255, -98.44999999890752918 ) ) ;
#3168 = VERTEX_POINT ( 'NONE', #2419 ) ;
#3169 = CARTESIAN_POINT ( 'NONE',  ( -22.97617564697422665, -31.74859572486943193, -7.102600956461224690 ) ) ;
#3170 = CARTESIAN_POINT ( 'NONE',  ( -28.38237549136062654, -32.45140427513058512, -9.857197362228843573 ) ) ;
#3171 = EDGE_LOOP ( 'NONE', ( #5856, #4703, #6154, #2983 ) ) ;
#3172 = CARTESIAN_POINT ( 'NONE',  ( -23.31994607974211675, -36.50140427513057517, 6.754974922286503869 ) ) ;
#3173 = CARTESIAN_POINT ( 'NONE',  ( -31.30653513488008244, -49.83744928702515864, 12.43572992548471845 ) ) ;
#3174 = DIRECTION ( 'NONE',  ( -0.000000000000000000, -0.000000000000000000, -1.000000000000000000 ) ) ;
#3175 = CARTESIAN_POINT ( 'NONE',  ( -3.535533905932736864, -41.46446609406723383, -97.39999999781504414 ) ) ;
#3176 = DIRECTION ( 'NONE',  ( -1.000000000000000000, 0.000000000000000000, 0.000000000000000000 ) ) ;
#3177 = CARTESIAN_POINT ( 'NONE',  ( -3.061616997868382155E-16, -39.99999999999997158, -97.60000000000000853 ) ) ;
#3178 = VERTEX_POINT ( 'NONE', #5259 ) ;
#3179 = CARTESIAN_POINT ( 'NONE',  ( -28.60187809025093841, -42.44999999999999574, -8.827394325379140483 ) ) ;
#3180 = EDGE_LOOP ( 'NONE', ( #1965, #2795, #5234, #6820 ) ) ;
#3181 = EDGE_CURVE ( 'NONE', #6859, #6385, #3292, .T. ) ;
#3182 = CARTESIAN_POINT ( 'NONE',  ( 5.000000000000000000, -47.07106781186545419, -97.85000000000002274 ) ) ;
#3183 = CARTESIAN_POINT ( 'NONE',  ( -4.581831634694143673, -42.91680744104596101, -100.0003077338198381 ) ) ;
#3184 = CARTESIAN_POINT ( 'NONE',  ( -34.00787565980851213, -35.15140427513058086, -7.988596311142238449 ) ) ;
#3185 = CARTESIAN_POINT ( 'NONE',  ( 39.85000000000002274, 21.99999999999992184, 80.00000000000002842 ) ) ;
#3186 = CARTESIAN_POINT ( 'NONE',  ( 50.00000000000002842, -44.99999999999997158, 0.000000000000000000 ) ) ;
#3187 = AXIS2_PLACEMENT_3D ( 'NONE', #5490, #7607, #8198 ) ;
#3188 = CARTESIAN_POINT ( 'NONE',  ( -31.32969295284206979, -39.30000000000001137, -8.395350895058669494 ) ) ;
#3189 = CARTESIAN_POINT ( 'NONE',  ( -30.00000000000000000, -45.00000000000000000, -30.00100000000000122 ) ) ;
#3190 = CARTESIAN_POINT ( 'NONE',  ( -39.38303923565386100, -50.70000000000000995, -1.486127417882099788 ) ) ;
#3191 = DIRECTION ( 'NONE',  ( 0.000000000000000000, -1.000000000000000000, 0.000000000000000000 ) ) ;
#3192 = VERTEX_POINT ( 'NONE', #1168 ) ;
#3193 = CARTESIAN_POINT ( 'NONE',  ( -33.81171626276147890, -48.09859572486944046, 7.597606577763319713 ) ) ;
#3194 = CARTESIAN_POINT ( 'NONE',  ( -34.53486167607238144, -39.14999999999999147, -8.900167166472096270 ) ) ;
#3195 = CARTESIAN_POINT ( 'NONE',  ( -38.38706344316003793, -40.70140427513058512, -1.382017864820032083 ) ) ;
#3196 = ADVANCED_FACE ( 'NONE', ( #7958, #7916 ), #5140, .F. ) ;
#3197 = CARTESIAN_POINT ( 'NONE',  ( 4.566987299999998307, -43.10829192115428299, -99.59999999890754907 ) ) ;
#3198 = MECHANICAL_DESIGN_GEOMETRIC_PRESENTATION_REPRESENTATION (  '', ( #4896 ), #6085 ) ;
#3199 = CARTESIAN_POINT ( 'NONE',  ( 45.00000000000003553, -44.99999999999997158, 0.000000000000000000 ) ) ;
#3200 = CARTESIAN_POINT ( 'NONE',  ( -20.14280263777121149, -41.04859572486944330, -1.617624508639600833 ) ) ;
#3201 = CARTESIAN_POINT ( 'NONE',  ( -21.53543802021056663, -39.90000000000000568, -4.312909747525783821 ) ) ;
#3202 = CARTESIAN_POINT ( 'NONE',  ( -4.999999999999998224, -44.99999999999997158, -98.89999999781504414 ) ) ;
#3203 = LINE ( 'NONE', #7912, #4711 ) ;
#3204 = CARTESIAN_POINT ( 'NONE',  ( 1.891708078845685481, -49.56698729999997255, -99.19999999890751496 ) ) ;
#3205 = ORIENTED_EDGE ( 'NONE', *, *, #4194, .F. ) ;
#3206 = CIRCLE ( 'NONE', #4048, 1.649999999999998579 ) ;
#3207 = CARTESIAN_POINT ( 'NONE',  ( -38.44051085762733777, -33.39859572486943762, 4.360112732550414982 ) ) ;
#3208 = CARTESIAN_POINT ( 'NONE',  ( -37.10260095646111012, -34.25140427513057517, 7.023824353025939438 ) ) ;
#3209 = AXIS2_PLACEMENT_3D ( 'NONE', #3288, #5964, #8083 ) ;
#3210 = EDGE_LOOP ( 'NONE', ( #5686, #3847 ) ) ;
#3211 = EDGE_LOOP ( 'NONE', ( #6063, #3558 ) ) ;
#3212 = CARTESIAN_POINT ( 'NONE',  ( -25.51477047955235378, -36.65140427513058086, 8.925456012876139766 ) ) ;
#3213 = DIRECTION ( 'NONE',  ( -0.000000000000000000, -0.000000000000000000, -1.000000000000000000 ) ) ;
#3214 = CARTESIAN_POINT ( 'NONE',  ( 2.071067811865477282, -49.99999999999997158, -97.15000000000000568 ) ) ;
#3215 = EDGE_CURVE ( 'NONE', #6557, #8668, #1881, .T. ) ;
#3216 = CARTESIAN_POINT ( 'NONE',  ( 9.184850993605145972E-16, -49.99999999999997158, -96.40000000000000568 ) ) ;
#3217 = DIRECTION ( 'NONE',  ( 0.000000000000000000, 0.000000000000000000, 1.000000000000000000 ) ) ;
#3218 = ORIENTED_EDGE ( 'NONE', *, *, #3900, .T. ) ;
#3219 = AXIS2_PLACEMENT_3D ( 'NONE', #3186, #7766, #2441 ) ;
#3220 = CARTESIAN_POINT ( 'NONE',  ( -22.03669253526174998, -40.35000000000000142, 4.057507815433014642 ) ) ;
#3221 = VERTEX_POINT ( 'NONE', #8495 ) ;
#3222 = CARTESIAN_POINT ( 'NONE',  ( 4.999999999999998224, -44.99999999999997158, -95.00000000000000000 ) ) ;
#3223 = EDGE_CURVE ( 'NONE', #580, #3619, #6583, .T. ) ;
#3224 = CARTESIAN_POINT ( 'NONE',  ( 2.071067811865477282, -49.99999999999996447, -97.15000000000000568 ) ) ;
#3225 = CARTESIAN_POINT ( 'NONE',  ( -39.38303923565386100, -32.70000000000000995, -1.486127417882099788 ) ) ;
#3226 = CARTESIAN_POINT ( 'NONE',  ( -7.654042494670954648E-16, -39.99999999999997158, -100.0000000000000000 ) ) ;
#3227 = CARTESIAN_POINT ( 'NONE',  ( -37.93801861833426159, -34.85140427513057659, -4.107139971057695682 ) ) ;
#3228 = DIRECTION ( 'NONE',  ( 1.049727191138618079E-16, 0.5150380749100549327, -0.8571673007021118895 ) ) ;
#3229 = CARTESIAN_POINT ( 'NONE',  ( -26.14108075221394856, -33.60000000000000142, -7.573555455601170827 ) ) ;
#3230 = EDGE_CURVE ( 'NONE', #1056, #6586, #1250, .T. ) ;
#3231 = DIRECTION ( 'NONE',  ( 0.000000000000000000, 0.000000000000000000, 1.000000000000000000 ) ) ;
#3232 = CARTESIAN_POINT ( 'NONE',  ( -20.61696076434619584, -46.20000000000000284, 1.486127417882100676 ) ) ;
#3233 = DIRECTION ( 'NONE',  ( 0.000000000000000000, 0.000000000000000000, 1.000000000000000000 ) ) ;
#3234 = ORIENTED_EDGE ( 'NONE', *, *, #3542, .F. ) ;
#3235 = CARTESIAN_POINT ( 'NONE',  ( -22.01140368885771892, -50.34859572486944046, 4.007875659808335378 ) ) ;
#3236 = CARTESIAN_POINT ( 'NONE',  ( -20.13408869516453947, -40.05000000000001137, -1.562606840307983136 ) ) ;
#3237 = CARTESIAN_POINT ( 'NONE',  ( -25.99212434019154472, -39.65140427513058086, 7.988596311142242890 ) ) ;
#3238 = CIRCLE ( 'NONE', #838, 7.499999999999999112 ) ;
#3239 = CARTESIAN_POINT ( 'NONE',  ( -30.00000000000019185, 0.000000000000000000, -40.35000000000000142 ) ) ;
#3240 = CARTESIAN_POINT ( 'NONE',  ( 2.000000000000000000, 1.773042676681340968, -1.951563910473907981E-15 ) ) ;
#3241 = CARTESIAN_POINT ( 'NONE',  ( -34.26570676250101855, -42.09859572486944046, 8.488613101951703044 ) ) ;
#3242 = CARTESIAN_POINT ( 'NONE',  ( -25.68709025247441602, -42.60000000000000853, -8.464561979789547053 ) ) ;
#3243 = CARTESIAN_POINT ( 'NONE',  ( 4.000000000000001776, 0.000000000000000000, -2.200000000000001066 ) ) ;
#3244 = DIRECTION ( 'NONE',  ( 0.000000000000000000, 0.000000000000000000, 1.000000000000000000 ) ) ;
#3245 = CARTESIAN_POINT ( 'NONE',  ( 4.566987300000000083, -46.89170807884565306, -96.49999999890752633 ) ) ;
#3246 =( NAMED_UNIT ( * ) PLANE_ANGLE_UNIT ( ) SI_UNIT ( $, .RADIAN. ) );
#3247 = AXIS2_PLACEMENT_3D ( 'NONE', #276, #7591, #6841 ) ;
#3248 = ORIENTED_EDGE ( 'NONE', *, *, #5233, .T. ) ;
#3249 = FACE_OUTER_BOUND ( 'NONE', #6089, .T. ) ;
#3250 = CARTESIAN_POINT ( 'NONE',  ( -37.98859631114233792, -48.84859572486942625, -4.007875659808334490 ) ) ;
#3251 = CARTESIAN_POINT ( 'NONE',  ( -39.37475178375516549, -34.70140427513057091, -1.538452329860249712 ) ) ;
#3252 = ORIENTED_EDGE ( 'NONE', *, *, #4497, .F. ) ;
#3253 = CARTESIAN_POINT ( 'NONE',  ( -34.36011273255026310, -43.10140427513058370, 8.440510857627391061 ) ) ;
#3254 = CARTESIAN_POINT ( 'NONE',  ( 3.535533969928884801, -41.46446615806338087, -100.0000000000000142 ) ) ;
#3255 = PLANE ( 'NONE',  #4115 ) ;
#3256 = CARTESIAN_POINT ( 'NONE',  ( 4.999999999999998224, -42.92893218813448897, -96.04999999781504982 ) ) ;
#3257 = CARTESIAN_POINT ( 'NONE',  ( 31.62245743458239033, -49.74093594125425000, 12.39808714042238869 ) ) ;
#3258 = CARTESIAN_POINT ( 'NONE',  ( -2.071067811865475061, -39.99999999999997158, -99.14999999999999147 ) ) ;
#3259 = EDGE_LOOP ( 'NONE', ( #3708, #7901 ) ) ;
#3260 = CIRCLE ( 'NONE', #7612, 1.649999999999998579 ) ;
#3261 = CARTESIAN_POINT ( 'NONE',  ( -31.39812190974910422, -37.94999999999998153, 8.827394325379140483 ) ) ;
#3262 = ADVANCED_FACE ( 'NONE', ( #3426 ), #2630, .F. ) ;
#3263 = ADVANCED_FACE ( 'NONE', ( #8702 ), #1308, .T. ) ;
#3264 = FACE_OUTER_BOUND ( 'NONE', #7296, .T. ) ;
#3265 = CARTESIAN_POINT ( 'NONE',  ( -3.229347689422840784, -41.77065231057713390, -95.54999999890752349 ) ) ;
#3266 = CARTESIAN_POINT ( 'NONE',  ( -4.999999999999998224, -44.99999999999997158, -96.49999999781503845 ) ) ;
#3267 = CARTESIAN_POINT ( 'NONE',  ( -28.43739315969223824, -42.44999999999999574, -9.865911304835512041 ) ) ;
#3268 = CARTESIAN_POINT ( 'NONE',  ( -4.566987299999998307, -43.10829192115428299, -99.29999999890752349 ) ) ;
#3269 = CARTESIAN_POINT ( 'NONE',  ( -4.864554114591847167, -46.28939218662745247, -100.0008501927092226 ) ) ;
#3270 = CARTESIAN_POINT ( 'NONE',  ( -35.97294713907137975, -38.00140427513057517, -6.047868141099968398 ) ) ;
#3271 = PRODUCT_DEFINITION_FORMATION_WITH_SPECIFIED_SOURCE ( 'ANY', '', #2345, .NOT_KNOWN. ) ;
#3272 = EDGE_CURVE ( 'NONE', #2422, #5583, #3112, .T. ) ;
#3273 = VECTOR ( 'NONE', #7798, 1000.000000000000000 ) ;
#3274 = CARTESIAN_POINT ( 'NONE',  ( -4.999999999999997335, -47.07106781186546129, -97.34300000002184561 ) ) ;
#3275 = CARTESIAN_POINT ( 'NONE',  ( -28.60187809025093841, -36.44999999999999574, -8.827394325379140483 ) ) ;
#3276 = LINE ( 'NONE', #658, #7565 ) ;
#3277 = EDGE_CURVE ( 'NONE', #1263, #2721, #6243, .T. ) ;
#3278 = CARTESIAN_POINT ( 'NONE',  ( -23.28248557872775137, -49.50000000000000711, 6.717514421272141156 ) ) ;
#3279 = DIRECTION ( 'NONE',  ( -1.000000000000000000, 0.000000000000000000, 0.000000000000000000 ) ) ;
#3280 = VERTEX_POINT ( 'NONE', #6716 ) ;
#3281 = DIRECTION ( 'NONE',  ( 0.000000000000000000, 0.000000000000000000, 1.000000000000000000 ) ) ;
#3282 = CARTESIAN_POINT ( 'NONE',  ( -22.93678734525658314, -33.75000000000001421, -7.063212654743582952 ) ) ;
#3283 = VECTOR ( 'NONE', #5938, 999.9999999999998863 ) ;
#3284 = CARTESIAN_POINT ( 'NONE',  ( -24.02705286092866643, -36.50140427513057517, 6.047868141099968398 ) ) ;
#3285 = VECTOR ( 'NONE', #6679, 1000.000000000000000 ) ;
#3286 = EDGE_CURVE ( 'NONE', #5904, #3178, #5474, .T. ) ;
#3287 = CARTESIAN_POINT ( 'NONE',  ( -4.566987299999998307, -44.99999999999997158, -95.34999999890753486 ) ) ;
#3288 = CARTESIAN_POINT ( 'NONE',  ( 4.200000000000001954, 0.000000000000000000, 0.000000000000000000 ) ) ;
#3289 = CARTESIAN_POINT ( 'NONE',  ( -38.92545601287626056, -33.84859572486942625, -4.485229520447501450 ) ) ;
#3290 = EDGE_CURVE ( 'NONE', #580, #3680, #8499, .T. ) ;
#3291 = DIRECTION ( 'NONE',  ( 1.000000000000000000, 0.000000000000000000, 0.000000000000000000 ) ) ;
#3292 = CIRCLE ( 'NONE', #8224, 12.49999999999997335 ) ;
#3293 = CARTESIAN_POINT ( 'NONE',  ( -3.061616997868382155E-16, -39.99999999999997158, -100.6999999978150555 ) ) ;
#3294 = CARTESIAN_POINT ( 'NONE',  ( -1.891708078845683039, -40.43301269999998482, -100.3999999989075178 ) ) ;
#3295 = SURFACE_SIDE_STYLE ('',( #2051 ) ) ;
#3296 = EDGE_LOOP ( 'NONE', ( #4294, #8539, #5437, #5285 ) ) ;
#3297 = CYLINDRICAL_SURFACE ( 'NONE', #888, 1.000000000000000888 ) ;
#3298 = CARTESIAN_POINT ( 'NONE',  ( -26.18828373723858149, -31.59859572486943335, -7.597606577763319713 ) ) ;
#3299 = CARTESIAN_POINT ( 'NONE',  ( -31.50758917197619979, -32.94859572486944188, 9.874625247442176956 ) ) ;
#3300 = CARTESIAN_POINT ( 'NONE',  ( -31.43380250590416125, -32.30140427513056522, -9.391326687552492558 ) ) ;
#3301 = ORIENTED_EDGE ( 'NONE', *, *, #4573, .T. ) ;
#3302 = CARTESIAN_POINT ( 'NONE',  ( -31.43380250590416125, -41.30140427513058654, -9.391326687552492558 ) ) ;
#3303 = CARTESIAN_POINT ( 'NONE',  ( 30.00000000000000000, 60.00000000000002842, 12.49999999999996625 ) ) ;
#3304 = CARTESIAN_POINT ( 'NONE',  ( 4.999999999999998224, -42.92893218813449607, -99.35000000000000853 ) ) ;
#3305 = CARTESIAN_POINT ( 'NONE',  ( -4.999999999999998224, -44.99999999999997158, -98.89999999781504414 ) ) ;
#3306 = CARTESIAN_POINT ( 'NONE',  ( 34.99999999999998579, -45.32948160161797091, 11.45643923738956893 ) ) ;
#3307 = CARTESIAN_POINT ( 'NONE',  ( -3.535533905932735532, -48.53553390593270933, -99.70000000000000284 ) ) ;
#3308 = AXIS2_PLACEMENT_3D ( 'NONE', #6496, #5711, #406 ) ;
#3309 = VERTEX_POINT ( 'NONE', #8185 ) ;
#3310 = CARTESIAN_POINT ( 'NONE',  ( -26.14108075221394856, -45.60000000000000853, -7.573555455601170827 ) ) ;
#3311 = EDGE_CURVE ( 'NONE', #3779, #3764, #8407, .T. ) ;
#3312 = ORIENTED_EDGE ( 'NONE', *, *, #3126, .T. ) ;
#3313 = CARTESIAN_POINT ( 'NONE',  ( -2.796473189345805913E-16, -40.43301269999997061, -98.84999999890752065 ) ) ;
#3314 = CARTESIAN_POINT ( 'NONE',  ( 2.071067811865474173, -39.99999999999997158, -96.74999999781503845 ) ) ;
#3315 = CARTESIAN_POINT ( 'NONE',  ( -34.31290974752564438, -44.10000000000000853, 8.464561979789547053 ) ) ;
#3316 = CARTESIAN_POINT ( 'NONE',  ( 8.389419568037416259E-16, -49.56698729999997255, -97.44999999890751496 ) ) ;
#3317 = CARTESIAN_POINT ( 'NONE',  ( 5.007363570061430735, -45.07891398322220056, -99.99974818118526798 ) ) ;
#3318 = CARTESIAN_POINT ( 'NONE',  ( -21.16389173201424612, -30.05140427513057944, -1.343104241417630185 ) ) ;
#3319 = CARTESIAN_POINT ( 'NONE',  ( -4.999999999999998224, -45.95670858091268940, -94.96990301170907856 ) ) ;
#3320 = AXIS2_PLACEMENT_3D ( 'NONE', #5224, #2510, #3872 ) ;
#3321 = CARTESIAN_POINT ( 'NONE',  ( -21.17260567462091103, -31.05000000000000426, -1.398121909749241887 ) ) ;
#3322 = CARTESIAN_POINT ( 'NONE',  ( 50.00000000000002842, 30.00000000000000000, 80.00000000000002842 ) ) ;
#3323 = EDGE_CURVE ( 'NONE', #6288, #6845, #674, .T. ) ;
#3324 = CARTESIAN_POINT ( 'NONE',  ( -36.71751442127229836, -51.00000000000000711, -6.717514421272142044 ) ) ;
#3325 = ORIENTED_EDGE ( 'NONE', *, *, #2305, .F. ) ;
#3326 = CYLINDRICAL_SURFACE ( 'NONE', #8419, 2.149999999999985256 ) ;
#3327 = CARTESIAN_POINT ( 'NONE',  ( -39.86591130483550671, -44.55000000000001137, 1.562606840307984468 ) ) ;
#3328 = CARTESIAN_POINT ( 'NONE',  ( -25.99212434019154472, -48.65140427513057375, 7.988596311142242890 ) ) ;
#3329 = CARTESIAN_POINT ( 'NONE',  ( -4.999999999999998224, -44.99999999999997158, -99.00000000000000000 ) ) ;
#3330 = CARTESIAN_POINT ( 'NONE',  ( -31.53845232986046554, -37.29859572486943620, -9.374751783755117529 ) ) ;
#3331 = DIRECTION ( 'NONE',  ( -0.000000000000000000, 1.000000000000000000, -0.000000000000000000 ) ) ;
#3332 = FACE_OUTER_BOUND ( 'NONE', #567, .T. ) ;
#3333 = CARTESIAN_POINT ( 'NONE',  ( 1.891708078845682595, -40.43301269999998482, -95.49999999890754054 ) ) ;
#3334 = SURFACE_STYLE_FILL_AREA ( #3990 ) ;
#3335 = ORIENTED_EDGE ( 'NONE', *, *, #2748, .F. ) ;
#3336 = CARTESIAN_POINT ( 'NONE',  ( 2.000000000000000000, 1.773042676681340968, -1.951563910473907981E-15 ) ) ;
#3337 = CARTESIAN_POINT ( 'NONE',  ( -28.67030704715798350, -49.80000000000001137, 8.395350895058669494 ) ) ;
#3338 = CARTESIAN_POINT ( 'NONE',  ( -23.24502507771338600, -38.49859572486943904, 6.680053920257780220 ) ) ;
#3339 = CARTESIAN_POINT ( 'NONE',  ( -31.61762450863942320, -36.95140427513057801, 9.857197362228843573 ) ) ;
#3340 = VECTOR ( 'NONE', #7589, 1000.000000000000000 ) ;
#3341 = ORIENTED_EDGE ( 'NONE', *, *, #2103, .F. ) ;
#3342 = ORIENTED_EDGE ( 'NONE', *, *, #6404, .T. ) ;
#3343 = CARTESIAN_POINT ( 'NONE',  ( -34.48522952044771017, -47.15140427513058086, -8.925456012876139766 ) ) ;
#3344 =( NAMED_UNIT ( * ) SI_UNIT ( $, .STERADIAN. ) SOLID_ANGLE_UNIT ( ) );
#3345 = CARTESIAN_POINT ( 'NONE',  ( -3.061616997868382155E-16, -39.99999999999997158, -99.20000000000000284 ) ) ;
#3346 = CARTESIAN_POINT ( 'NONE',  ( 4.999999999999998224, -42.92893218813448897, -100.0499999978150356 ) ) ;
#3347 = LINE ( 'NONE', #5268, #6368 ) ;
#3348 = CARTESIAN_POINT ( 'NONE',  ( 4.999999999999998224, -44.99999999999997158, -98.60000000000000853 ) ) ;
#3349 = ADVANCED_FACE ( 'NONE', ( #5970 ), #1428, .F. ) ;
#3350 = ORIENTED_EDGE ( 'NONE', *, *, #1007, .T. ) ;
#3351 = AXIS2_PLACEMENT_3D ( 'NONE', #5922, #5380, #1913 ) ;
#3352 = CARTESIAN_POINT ( 'NONE',  ( -23.98959235991431171, -46.50000000000000711, 6.010407640085604797 ) ) ;
#3353 = CARTESIAN_POINT ( 'NONE',  ( -20.13408869516453947, -34.04999999999998295, -1.562606840307983136 ) ) ;
#3354 = VECTOR ( 'NONE', #8380, 1000.000000000000000 ) ;
#3355 = CARTESIAN_POINT ( 'NONE',  ( -30.00000000000000000, 0.000000000000000000, 80.00000000000002842 ) ) ;
#3356 = CARTESIAN_POINT ( 'NONE',  ( -4.566987299999998307, -44.99999999999997158, -98.64999999890751781 ) ) ;
#3357 = CARTESIAN_POINT ( 'NONE',  ( -3.535533905932735532, -48.53553390593270933, -99.70000000000000284 ) ) ;
#3358 = CARTESIAN_POINT ( 'NONE',  ( -23.28248557872775137, -43.50000000000001421, 6.717514421272141156 ) ) ;
#3359 = CARTESIAN_POINT ( 'NONE',  ( 4.566987300000000083, -46.89170807884565306, -98.89999999890753202 ) ) ;
#3360 = APPLICATION_CONTEXT ( 'automotive_design' ) ;
#3361 = CARTESIAN_POINT ( 'NONE',  ( -34.35889894354067309, 8.000000000000000000, 125.0000000000000000 ) ) ;
#3362 = CARTESIAN_POINT ( 'NONE',  ( -37.59760657776328685, -34.40140427513058086, 3.811716262761598362 ) ) ;
#3363 = CARTESIAN_POINT ( 'NONE',  ( 2.071067811865474173, -39.99999999999997158, -96.84300000002187403 ) ) ;
#3364 = CARTESIAN_POINT ( 'NONE',  ( -38.39535089505872634, -35.70000000000000995, -1.329692952841885267 ) ) ;
#3365 = CARTESIAN_POINT ( 'NONE',  ( 2.071067811865474173, -39.99999999999997158, -97.65000000000000568 ) ) ;
#3366 = CARTESIAN_POINT ( 'NONE',  ( -30.00000000000002842, 0.000000000000000000, -26.00000000000000355 ) ) ;
#3367 = CARTESIAN_POINT ( 'NONE',  ( 0.000000000000000000, 0.000000000000000000, 0.000000000000000000 ) ) ;
#3368 = EDGE_LOOP ( 'NONE', ( #3693, #8359, #249, #3301 ) ) ;
#3369 = CARTESIAN_POINT ( 'NONE',  ( -5.000000000000007105, -47.07106781186543998, -99.74999999999998579 ) ) ;
#3370 = CARTESIAN_POINT ( 'NONE',  ( -38.46456197978948666, -44.40000000000000568, 4.312909747525784709 ) ) ;
#3371 = CARTESIAN_POINT ( 'NONE',  ( -23.64089511245930098, -47.75140427513058938, -6.280328284105564762 ) ) ;
#3372 = CARTESIAN_POINT ( 'NONE',  ( -4.999999999999998224, -44.99999999999997158, -96.60000000000000853 ) ) ;
#3373 = CYLINDRICAL_SURFACE ( 'NONE', #4324, 11.99999999999979217 ) ;
#3374 = CARTESIAN_POINT ( 'NONE',  ( -25.73429323749904185, -46.59859572486944046, -8.488613101951701267 ) ) ;
#3375 = EDGE_CURVE ( 'NONE', #912, #2594, #6672, .T. ) ;
#3376 = DIRECTION ( 'NONE',  ( 0.000000000000000000, 0.000000000000000000, 1.000000000000000000 ) ) ;
#3377 = DIRECTION ( 'NONE',  ( -0.000000000000000000, -0.000000000000000000, -1.000000000000000000 ) ) ;
#3378 = CARTESIAN_POINT ( 'NONE',  ( -2.796473189345805913E-16, -40.43301269999997061, -96.24999999890752633 ) ) ;
#3379 = VERTEX_POINT ( 'NONE', #6014 ) ;
#3380 = CARTESIAN_POINT ( 'NONE',  ( -50.00000000000002842, 30.00000000000000000, 80.00000000000002842 ) ) ;
#3381 = CARTESIAN_POINT ( 'NONE',  ( -23.71967171589458445, -31.74859572486943193, -6.359104887540838469 ) ) ;
#3382 = CARTESIAN_POINT ( 'NONE',  ( -21.07454398712378918, -41.34859572486944757, 4.485229520447505003 ) ) ;
#3383 = CARTESIAN_POINT ( 'NONE',  ( -37.10260095646111012, -37.25140427513058228, 7.023824353025939438 ) ) ;
#3384 = EDGE_CURVE ( 'NONE', #5890, #7483, #4317, .T. ) ;
#3385 = ORIENTED_EDGE ( 'NONE', *, *, #5412, .F. ) ;
#3386 = ORIENTED_EDGE ( 'NONE', *, *, #6404, .F. ) ;
#3387 = CARTESIAN_POINT ( 'NONE',  ( -31.43380250590416125, -47.30140427513057944, -9.391326687552492558 ) ) ;
#3388 = CARTESIAN_POINT ( 'NONE',  ( -2.796473189345805913E-16, -40.43301269999997061, -100.2499999989075263 ) ) ;
#3389 = CARTESIAN_POINT ( 'NONE',  ( 4.999999999999998224, -44.99999999999997158, -99.40000000000000568 ) ) ;
#3390 = AXIS2_PLACEMENT_3D ( 'NONE', #2932, #5605, #5427 ) ;
#3391 = CARTESIAN_POINT ( 'NONE',  ( 2.071067811865474173, -39.99999999999997158, -98.34999999781506119 ) ) ;
#3392 = CARTESIAN_POINT ( 'NONE',  ( 50.00000000000002842, 60.00000000000002842, 30.00000000000000000 ) ) ;
#3393 = CARTESIAN_POINT ( 'NONE',  ( 9.184850993605145972E-16, -49.99999999999997158, -99.59999999999999432 ) ) ;
#3394 = VERTEX_POINT ( 'NONE', #4698 ) ;
#3395 = EDGE_CURVE ( 'NONE', #4958, #899, #3058, .T. ) ;
#3396 = CARTESIAN_POINT ( 'NONE',  ( -21.59636165304264921, -35.19859572486944188, 1.277368040863740228 ) ) ;
#3397 = CARTESIAN_POINT ( 'NONE',  ( -34.31290974752564438, -38.10000000000000853, 8.464561979789547053 ) ) ;
#3398 = ORIENTED_EDGE ( 'NONE', *, *, #7019, .F. ) ;
#3399 = CARTESIAN_POINT ( 'NONE',  ( 1.891708078845685481, -49.56698729999997255, -97.59999999890753486 ) ) ;
#3400 = CARTESIAN_POINT ( 'NONE',  ( -4.999999999999998224, -42.92893218813448897, -96.54999999781504982 ) ) ;
#3401 = CARTESIAN_POINT ( 'NONE',  ( -39.86591130483550671, -44.55000000000001137, 1.562606840307984468 ) ) ;
#3402 = CARTESIAN_POINT ( 'NONE',  ( 1.891708078845682595, -40.43301269999998482, -97.89999999890753202 ) ) ;
#3403 = EDGE_CURVE ( 'NONE', #8652, #7915, #8265, .T. ) ;
#3404 = CARTESIAN_POINT ( 'NONE',  ( -38.83610826798580717, -40.55140427513058654, 1.343104241417631073 ) ) ;
#3405 = COLOUR_RGB ( '', 0.08235294, 0.09019608, 0.10196078) ;
#3406 = CARTESIAN_POINT ( 'NONE',  ( 4.999999999999998224, -44.99999999999997158, -96.99300000002185129 ) ) ;
#3407 = CARTESIAN_POINT ( 'NONE',  ( -22.03669253526174998, -46.34999999999999432, 4.057507815433014642 ) ) ;
#3408 = CARTESIAN_POINT ( 'NONE',  ( -30.00000000000002487, 0.000000000000000000, -41.35000000000000142 ) ) ;
#3409 = PRODUCT_DEFINITION_FORMATION_WITH_SPECIFIED_SOURCE ( 'ANY', '', #7676, .NOT_KNOWN. ) ;
#3410 = CARTESIAN_POINT ( 'NONE',  ( 2.071067811865474173, -39.99999999999997158, -95.94999999781504130 ) ) ;
#3411 = ADVANCED_FACE ( 'NONE', ( #5432 ), #4592, .F. ) ;
#3412 = ORIENTED_EDGE ( 'NONE', *, *, #4868, .F. ) ;
#3413 = DIRECTION ( 'NONE',  ( -1.000000000000000000, -0.000000000000000000, -0.000000000000000000 ) ) ;
#3414 = CARTESIAN_POINT ( 'NONE',  ( -23.28248557872775137, -46.50000000000000711, 6.717514421272141156 ) ) ;
#3415 = CARTESIAN_POINT ( 'NONE',  ( -36.01040764008574513, -30.00000000000000711, -6.010407640085605685 ) ) ;
#3416 = ADVANCED_FACE ( 'NONE', ( #3467 ), #792, .T. ) ;
#3417 = AXIS2_PLACEMENT_3D ( 'NONE', #2887, #933, #3626 ) ;
#3418 = FACE_BOUND ( 'NONE', #293, .T. ) ;
#3419 = CARTESIAN_POINT ( 'NONE',  ( 0.000000000000000000, 0.000000000000000000, 0.000000000000000000 ) ) ;
#3420 = CARTESIAN_POINT ( 'NONE',  ( -28.46154767013959486, -50.79859572486945041, 9.374751783755112200 ) ) ;
#3421 = CARTESIAN_POINT ( 'NONE',  ( 42.00000000000000711, 60.00000000000002842, 21.99999999999992184 ) ) ;
#3422 = CARTESIAN_POINT ( 'NONE',  ( -25.68709025247441602, -33.60000000000000142, -8.464561979789547053 ) ) ;
#3424 = CONICAL_SURFACE ( 'NONE', #7921, 1.649999999999998579, 1.029744258676653645 ) ;
#3423 =( LENGTH_UNIT ( ) NAMED_UNIT ( * ) SI_UNIT ( .MILLI., .METRE. ) );
#3425 = EDGE_LOOP ( 'NONE', ( #6570, #4915, #3398, #5999 ) ) ;
#3426 = FACE_OUTER_BOUND ( 'NONE', #8050, .T. ) ;
#3427 = CARTESIAN_POINT ( 'NONE',  ( -36.04786814110010340, -30.99859572486944259, -5.972947139071243861 ) ) ;
#3428 = CARTESIAN_POINT ( 'NONE',  ( -38.92545601287626056, -39.84859572486944046, -4.485229520447501450 ) ) ;
#3429 = CARTESIAN_POINT ( 'NONE',  ( -20.62524821624488069, -42.20140427513058512, 1.538452329860250378 ) ) ;
#3430 = ORIENTED_EDGE ( 'NONE', *, *, #3749, .F. ) ;
#3431 = VERTEX_POINT ( 'NONE', #6056 ) ;
#3432 = CARTESIAN_POINT ( 'NONE',  ( -38.87487832006816291, -40.85140427513057659, -4.584493831696867971 ) ) ;
#3433 = STYLED_ITEM ( 'NONE', ( #7390 ), #2885 ) ;
#3434 =( NAMED_UNIT ( * ) SI_UNIT ( $, .STERADIAN. ) SOLID_ANGLE_UNIT ( ) );
#3435 = LINE ( 'NONE', #6110, #8616 ) ;
#3436 = CARTESIAN_POINT ( 'NONE',  ( 4.566987299999998307, -43.10829192115428299, -95.79999999890752349 ) ) ;
#3437 = DIRECTION ( 'NONE',  ( 0.000000000000000000, 0.8660254037844380415, -0.5000000000000012212 ) ) ;
#3438 = DIRECTION ( 'NONE',  ( 0.000000000000000000, 0.000000000000000000, 1.000000000000000000 ) ) ;
#3439 = VERTEX_POINT ( 'NONE', #941 ) ;
#3440 = CARTESIAN_POINT ( 'NONE',  ( -21.18131961722757595, -32.04859572486944330, -1.453139578080854699 ) ) ;
#3441 = CARTESIAN_POINT ( 'NONE',  ( -39.38303923565386100, -38.70000000000000284, -1.486127417882099788 ) ) ;
#3442 = ORIENTED_EDGE ( 'NONE', *, *, #6773, .T. ) ;
#3443 = CARTESIAN_POINT ( 'NONE',  ( -40.00000000000002842, 1.224646799147353059E-15, -29.65000000000000213 ) ) ;
#3444 = CARTESIAN_POINT ( 'NONE',  ( -2.796473189345805913E-16, -40.43301269999997061, -96.44999999890751496 ) ) ;
#3445 = AXIS2_PLACEMENT_3D ( 'NONE', #534, #4645, #3244 ) ;
#3446 = CARTESIAN_POINT ( 'NONE',  ( -3.061616997868382155E-16, -39.99999999999997158, -96.69999999781504130 ) ) ;
#3447 = CARTESIAN_POINT ( 'NONE',  ( -38.90016716647221529, -47.85000000000000853, -4.534861676072185155 ) ) ;
#3448 = CARTESIAN_POINT ( 'NONE',  ( 4.566987299999998307, -44.99999999999997158, -98.04999999890752349 ) ) ;
#3449 = CARTESIAN_POINT ( 'NONE',  ( -22.40239342223677355, -47.90140427513058086, -3.811716262761597473 ) ) ;
#3450 = SHAPE_REPRESENTATION ( 'o-rings series a_iso_O-ring 20x2.65-A-ISO 3601-1', ( #2554 ), #1004 ) ;
#3451 = EDGE_CURVE ( 'NONE', #505, #4683, #2277, .T. ) ;
#3452 = CARTESIAN_POINT ( 'NONE',  ( -3.535533905932735532, -48.53553390593270933, -96.49300000002185129 ) ) ;
#3453 = UNCERTAINTY_MEASURE_WITH_UNIT (LENGTH_MEASURE( 1.000000000000000082E-05 ), #4314, 'distance_accuracy_value', 'NONE');
#3454 = CARTESIAN_POINT ( 'NONE',  ( -26.14108075221394856, -48.60000000000000142, -7.573555455601170827 ) ) ;
#3455 = DIRECTION ( 'NONE',  ( 0.000000000000000000, 0.000000000000000000, -1.000000000000000000 ) ) ;
#3456 = APPLICATION_PROTOCOL_DEFINITION ( 'draft international standard', 'automotive_design', 1998, #7404 ) ;
#3457 = EDGE_LOOP ( 'NONE', ( #1896, #5800, #5419 ) ) ;
#3458 = FACE_OUTER_BOUND ( 'NONE', #8186, .T. ) ;
#3459 = CARTESIAN_POINT ( 'NONE',  ( -34.31290974752564438, -50.10000000000000853, 8.464561979789547053 ) ) ;
#3460 = CARTESIAN_POINT ( 'NONE',  ( -23.98959235991431171, -31.50000000000000711, 6.010407640085604797 ) ) ;
#3461 = DIRECTION ( 'NONE',  ( 0.000000000000000000, 0.000000000000000000, 1.000000000000000000 ) ) ;
#3462 = LINE ( 'NONE', #6184, #3753 ) ;
#3463 = CARTESIAN_POINT ( 'NONE',  ( -21.55948914237271907, -46.89859572486944472, -4.360112732550413206 ) ) ;
#3464 = LINE ( 'NONE', #6145, #5777 ) ;
#3465 = CARTESIAN_POINT ( 'NONE',  ( -25.68709025247441602, -30.60000000000000142, -8.464561979789547053 ) ) ;
#3466 = VERTEX_POINT ( 'NONE', #6976 ) ;
#3467 = FACE_OUTER_BOUND ( 'NONE', #7873, .T. ) ;
#3468 = ORIENTED_EDGE ( 'NONE', *, *, #5047, .F. ) ;
#3469 = CIRCLE ( 'NONE', #5012, 4.999999999999998224 ) ;
#3470 = CARTESIAN_POINT ( 'NONE',  ( -31.38201786482021305, -34.29859572486943620, -8.387063443159975762 ) ) ;
#3471 = CARTESIAN_POINT ( 'NONE',  ( -36.75497492228666374, -42.99859572486943904, -6.680053920257780220 ) ) ;
#3472 = CARTESIAN_POINT ( 'NONE',  ( -38.48861310195163554, -40.40140427513058086, 4.265706762501153548 ) ) ;
#3473 = ORIENTED_EDGE ( 'NONE', *, *, #8303, .T. ) ;
#3474 =( REPRESENTATION_RELATIONSHIP ('NONE','NONE', #2265, #7097 ) REPRESENTATION_RELATIONSHIP_WITH_TRANSFORMATION ( #3097 )SHAPE_REPRESENTATION_RELATIONSHIP( ) );
#3475 = ORIENTED_EDGE ( 'NONE', *, *, #395, .T. ) ;
#3476 = CARTESIAN_POINT ( 'NONE',  ( -4.566987299999998307, -43.10829192115428299, -95.29999999890752349 ) ) ;
#3477 = CARTESIAN_POINT ( 'NONE',  ( -31.31024842726172608, -40.16330870357086980, 12.43543189630224077 ) ) ;
#3478 = CARTESIAN_POINT ( 'NONE',  ( -3.229347689422839451, -48.22934768942280925, -98.54999999890752349 ) ) ;
#3479 = CARTESIAN_POINT ( 'NONE',  ( 0.000000000000000000, -44.99999999999997158, -105.0000000000000142 ) ) ;
#3480 = CARTESIAN_POINT ( 'NONE',  ( -4.999999999999998224, -44.99999999999997158, -96.49999999781503845 ) ) ;
#3481 = ORIENTED_EDGE ( 'NONE', *, *, #3290, .T. ) ;
#3482 = VECTOR ( 'NONE', #4649, 1000.000000000000000 ) ;
#3483 = CARTESIAN_POINT ( 'NONE',  ( -23.95213185889994989, -35.49859572486943193, 5.972947139071243861 ) ) ;
#3484 = CARTESIAN_POINT ( 'NONE',  ( -28.51387258211773812, -34.80000000000000426, 9.383039235653802379 ) ) ;
#3485 = AXIS2_PLACEMENT_3D ( 'NONE', #1327, #5920, #4028 ) ;
#3486 = ORIENTED_EDGE ( 'NONE', *, *, #5192, .F. ) ;
#3487 = CARTESIAN_POINT ( 'NONE',  ( -31.56260684030781505, -46.94999999999998863, 9.865911304835510265 ) ) ;
#3488 = CARTESIAN_POINT ( 'NONE',  ( -1.891708078845683705, -49.56698729999997255, -96.89999999890753202 ) ) ;
#3489 = CARTESIAN_POINT ( 'NONE',  ( -4.999999999999998224, -42.92893218813448897, -100.5499999978150498 ) ) ;
#3490 = CARTESIAN_POINT ( 'NONE',  ( -39.86591130483550671, -50.55000000000001137, 1.562606840307984468 ) ) ;
#3491 = CARTESIAN_POINT ( 'NONE',  ( 3.229347689422841228, -48.22934768942280925, -97.34999999890753486 ) ) ;
#3492 = LINE ( 'NONE', #3649, #7759 ) ;
#3493 = CARTESIAN_POINT ( 'NONE',  ( -28.72263195913613387, -45.80140427513057944, 8.403638346957361449 ) ) ;
#3494 = CIRCLE ( 'NONE', #240, 9.999999999999994671 ) ;
#3495 = EDGE_CURVE ( 'NONE', #7164, #6529, #645, .T. ) ;
#3496 = CARTESIAN_POINT ( 'NONE',  ( -3.535533905932736864, -41.46446609406723383, -95.10000000000000853 ) ) ;
#3497 = CARTESIAN_POINT ( 'NONE',  ( -38.82739432537914581, -47.55000000000000426, 1.398121909749243663 ) ) ;
#3498 = DIRECTION ( 'NONE',  ( 1.000000000000000000, 0.000000000000000000, 0.000000000000000000 ) ) ;
#3499 =( BOUNDED_SURFACE ( )  B_SPLINE_SURFACE ( 1, 2, ( 
 ( #5071, #7055, #2310, #8390, #5776, #7671, #547, #3256, #4944, #6306, #5031, #8343, #5643, #2262, #1774, #2351, #2968, #7624, #8472, #311, #6347, #1589, #3013, #348, #7762, #930, #7809, #3056, #1634, #8301, #7721, #5688, #389, #5733, #1729, #4328, #3623, #4370, #1015, #7009, #972, #4455, #6391, #3667, #4415, #7101, #1058, #3751, #6436, #2435, #4708, #8013, #5267, #3391, #2685, #1258, #5979, #26, #592, #5352, #4749, #775, #2064, #5397, #3305, #6814, #6067, #2727, #1346, #7477, #2641, #1440, #6633, #1931, #8672, #5312, #5937, #4133, #8106, #1970, #5440, #8055, #7968, #4045, #6765, #2112, #4658, #3346, #2598, #6023, #4617, #8712, #7346, #3956, #8631, #2019, #729, #6726, #7392, #7301, #1302 ),
 ( #685, #4001, #6681, #7436, #1393, #639, #4089, #3436, #6111, #68, #2775, #8153, #4794, #8196, #5575, #5010, #2816, #2156, #245, #4841, #6160, #7699, #289, #4967, #4262, #4174, #117, #4883, #2244, #7604, #6900, #6856, #7520, #1659, #908, #1613, #2860, #1523, #821, #5488, #1480, #8369, #6987, #2331, #1566, #4923, #951, #4350, #3603, #5535, #6324, #3521, #861, #6944, #6284, #6247, #6199, #3646, #2990, #2946, #7030, #5666, #3478, #163, #8240, #2198, #5621, #7561, #4217, #8323, #3563, #2285, #204, #2906, #8283, #7650, #4302, #8529, #8489, #6369, #4435, #5093, #3814, #1833, #4515, #7827, #2415, #5710, #3118, #2536, #330, #8412, #6495, #2376, #3689, #5215, #6537, #2495, #1792, #1704, #3036 ) ),
 .UNSPECIFIED., .F., .F., .T. ) 
 B_SPLINE_SURFACE_WITH_KNOTS ( ( 2, 2 ),
 ( 3, 2, 2, 2, 2, 2, 2, 2, 2, 2, 2, 2, 2, 2, 2, 2, 2, 2, 2, 2, 2, 2, 2, 2, 2, 2, 2, 2, 2, 2, 2, 2, 2, 2, 2, 2, 2, 2, 2, 2, 2, 2, 2, 2, 2, 2, 2, 2, 2, 2, 3 ),
 ( 0.000000000000000000, 1.000000000000000000 ),
 ( 0.000000000000000000, 0.01785714285714285615, 0.03571428571428571230, 0.05357142857142856845, 0.07142857142857142461, 0.08928571428571428770, 0.1071428571428571369, 0.1250000000000000000, 0.1428571428571428492, 0.1607142857142857262, 0.1785714285714285754, 0.1964285714285714246, 0.2142857142857142738, 0.2321428571428571508, 0.2500000000000000000, 0.2678571428571428492, 0.2857142857142856984, 0.3035714285714285476, 0.3214285714285714524, 0.3392857142857143016, 0.3571428571428571508, 0.3750000000000000000, 0.3928571428571428492, 0.4107142857142856984, 0.4285714285714285476, 0.4464285714285714524, 0.4642857142857143016, 0.4821428571428571508, 0.5000000000000000000, 0.5178571428571429047, 0.5357142857142856984, 0.5535714285714286031, 0.5714285714285713969, 0.5892857142857143016, 0.6071428571428570953, 0.6250000000000000000, 0.6428571428571429047, 0.6607142857142856984, 0.6785714285714286031, 0.6964285714285713969, 0.7142857142857143016, 0.7321428571428570953, 0.7500000000000000000, 0.7678571428571429047, 0.7857142857142856984, 0.8035714285714286031, 0.8214285714285713969, 0.8392857142857143016, 0.8571428571428570953, 0.8750000000000000000, 0.8928571428571429047 ),
 .UNSPECIFIED. ) 
 GEOMETRIC_REPRESENTATION_ITEM ( )  RATIONAL_B_SPLINE_SURFACE ( (
 ( 1.000000000000000000, 0.9238795325112867385, 1.000000000000000000, 0.9238795325112867385, 1.000000000000000000, 0.9238795325112867385, 1.000000000000000000, 0.9238795325112867385, 1.000000000000000000, 0.9238795325112867385, 1.000000000000000000, 0.9238795325112867385, 1.000000000000000000, 0.9238795325112867385, 1.000000000000000000, 0.9238795325112867385, 1.000000000000000000, 0.9238795325112867385, 1.000000000000000000, 0.9238795325112867385, 1.000000000000000000, 0.9238795325112867385, 1.000000000000000000, 0.9238795325112867385, 1.000000000000000000, 0.9238795325112867385, 1.000000000000000000, 0.9238795325112867385, 1.000000000000000000, 0.9238795325112867385, 1.000000000000000000, 0.9238795325112867385, 1.000000000000000000, 0.9238795325112867385, 1.000000000000000000, 0.9238795325112867385, 1.000000000000000000, 0.9238795325112867385, 1.000000000000000000, 0.9238795325112867385, 1.000000000000000000, 0.9238795325112867385, 1.000000000000000000, 0.9238795325112867385, 1.000000000000000000, 0.9238795325112867385, 1.000000000000000000, 0.9238795325112867385, 1.000000000000000000, 0.9238795325112867385, 1.000000000000000000, 0.9238795325112867385, 1.000000000000000000, 0.9238795325112867385, 1.000000000000000000, 0.9238795325112867385, 1.000000000000000000, 0.9238795325112867385, 1.000000000000000000, 0.9238795325112867385, 1.000000000000000000, 0.9238795325112867385, 1.000000000000000000, 0.9238795325112867385, 1.000000000000000000, 0.9238795325112867385, 1.000000000000000000, 0.9238795325112867385, 1.000000000000000000, 0.9238795325112867385, 1.000000000000000000, 0.9238795325112867385, 1.000000000000000000, 0.9238795325112867385, 1.000000000000000000, 0.9238795325112867385, 1.000000000000000000, 0.9238795325112867385, 1.000000000000000000, 0.9238795325112867385, 1.000000000000000000, 0.9238795325112867385, 1.000000000000000000, 0.9238795325112867385, 1.000000000000000000, 0.9238795325112867385, 1.000000000000000000, 0.9238795325112867385, 1.000000000000000000, 0.9238795325112867385, 1.000000000000000000, 0.9238795325112867385, 1.000000000000000000, 0.9238795325112867385, 1.000000000000000000, 0.9238795325112867385, 1.000000000000000000, 0.9238795325112867385, 1.000000000000000000, 0.9238795325112867385, 1.000000000000000000),
 ( 1.000000000000000000, 0.9238795325112867385, 1.000000000000000000, 0.9238795325112867385, 1.000000000000000000, 0.9238795325112867385, 1.000000000000000000, 0.9238795325112867385, 1.000000000000000000, 0.9238795325112867385, 1.000000000000000000, 0.9238795325112867385, 1.000000000000000000, 0.9238795325112867385, 1.000000000000000000, 0.9238795325112867385, 1.000000000000000000, 0.9238795325112867385, 1.000000000000000000, 0.9238795325112867385, 1.000000000000000000, 0.9238795325112867385, 1.000000000000000000, 0.9238795325112867385, 1.000000000000000000, 0.9238795325112867385, 1.000000000000000000, 0.9238795325112867385, 1.000000000000000000, 0.9238795325112867385, 1.000000000000000000, 0.9238795325112867385, 1.000000000000000000, 0.9238795325112867385, 1.000000000000000000, 0.9238795325112867385, 1.000000000000000000, 0.9238795325112867385, 1.000000000000000000, 0.9238795325112867385, 1.000000000000000000, 0.9238795325112867385, 1.000000000000000000, 0.9238795325112867385, 1.000000000000000000, 0.9238795325112867385, 1.000000000000000000, 0.9238795325112867385, 1.000000000000000000, 0.9238795325112867385, 1.000000000000000000, 0.9238795325112867385, 1.000000000000000000, 0.9238795325112867385, 1.000000000000000000, 0.9238795325112867385, 1.000000000000000000, 0.9238795325112867385, 1.000000000000000000, 0.9238795325112867385, 1.000000000000000000, 0.9238795325112867385, 1.000000000000000000, 0.9238795325112867385, 1.000000000000000000, 0.9238795325112867385, 1.000000000000000000, 0.9238795325112867385, 1.000000000000000000, 0.9238795325112867385, 1.000000000000000000, 0.9238795325112867385, 1.000000000000000000, 0.9238795325112867385, 1.000000000000000000, 0.9238795325112867385, 1.000000000000000000, 0.9238795325112867385, 1.000000000000000000, 0.9238795325112867385, 1.000000000000000000, 0.9238795325112867385, 1.000000000000000000, 0.9238795325112867385, 1.000000000000000000, 0.9238795325112867385, 1.000000000000000000, 0.9238795325112867385, 1.000000000000000000, 0.9238795325112867385, 1.000000000000000000, 0.9238795325112867385, 1.000000000000000000, 0.9238795325112867385, 1.000000000000000000, 0.9238795325112867385, 1.000000000000000000, 0.9238795325112867385, 1.000000000000000000, 0.9238795325112867385, 1.000000000000000000) ) ) 
 REPRESENTATION_ITEM ( '' )  SURFACE ( )  );
#3500 = APPLICATION_PROTOCOL_DEFINITION ( 'draft international standard', 'automotive_design', 1998, #4368 ) ;
#3501 = ORIENTED_EDGE ( 'NONE', *, *, #1007, .F. ) ;
#3502 = SURFACE_STYLE_USAGE ( .BOTH. , #8347 ) ;
#3503 = CARTESIAN_POINT ( 'NONE',  ( -38.90016716647221529, -50.84999999999999432, -4.534861676072185155 ) ) ;
#3504 = CARTESIAN_POINT ( 'NONE',  ( -21.17260567462091458, -37.05000000000001137, -1.398121909749242331 ) ) ;
#3505 = EDGE_CURVE ( 'NONE', #4829, #1713, #151, .T. ) ;
#3506 = CARTESIAN_POINT ( 'NONE',  ( -26.69211319910860070, -41.23645700522185820, 12.05676622698253730 ) ) ;
#3507 = CARTESIAN_POINT ( 'NONE',  ( 34.00000000000000000, 1.971681346627238735E-16, -1.610000000000000098 ) ) ;
#3508 = CARTESIAN_POINT ( 'NONE',  ( -34.58449383169706692, -43.14859572486943762, -8.874878320068054549 ) ) ;
#3509 = CARTESIAN_POINT ( 'NONE',  ( 50.00000000000002842, 30.00000000000000000, 60.00000000000002842 ) ) ;
#3510 = CARTESIAN_POINT ( 'NONE',  ( -4.999999999999997335, -47.07106781186546129, -99.64999999781505835 ) ) ;
#3511 = EDGE_LOOP ( 'NONE', ( #7176, #8576, #8707 ) ) ;
#3512 = DIRECTION ( 'NONE',  ( -0.000000000000000000, 1.000000000000000000, -0.000000000000000000 ) ) ;
#3513 = EDGE_LOOP ( 'NONE', ( #7235, #1382 ) ) ;
#3514 = CARTESIAN_POINT ( 'NONE',  ( -33.81171626276147890, -36.09859572486943335, 7.597606577763319713 ) ) ;
#3515 = CARTESIAN_POINT ( 'NONE',  ( -20.60867331244750034, -44.19859572486944899, 1.433802505903951419 ) ) ;
#3516 = CARTESIAN_POINT ( 'NONE',  ( -25.51477047955235378, -42.65140427513058086, 8.925456012876139766 ) ) ;
#3517 = EDGE_LOOP ( 'NONE', ( #1012, #5611 ) ) ;
#3518 = CARTESIAN_POINT ( 'NONE',  ( 4.566987299999998307, -44.99999999999997158, -97.24999999890752633 ) ) ;
#3519 = SURFACE_SIDE_STYLE ('',( #202 ) ) ;
#3520 = DIRECTION ( 'NONE',  ( 1.049727191138618079E-16, 0.5150380749100549327, -0.8571673007021118895 ) ) ;
#3521 = CARTESIAN_POINT ( 'NONE',  ( -1.891708078845683039, -40.43301269999998482, -97.99999999890752633 ) ) ;
#3522 = DIRECTION ( 'NONE',  ( -1.000000000000000000, -0.000000000000000000, -0.000000000000000000 ) ) ;
#3523 = DIRECTION ( 'NONE',  ( -0.000000000000000000, 1.000000000000000000, -0.000000000000000000 ) ) ;
#3524 = ORIENTED_EDGE ( 'NONE', *, *, #926, .T. ) ;
#3525 = CARTESIAN_POINT ( 'NONE',  ( -21.60464910494133406, -49.20000000000000995, 1.329692952841886155 ) ) ;
#3526 = CARTESIAN_POINT ( 'NONE',  ( -21.53543802021056663, -30.90000000000000924, -4.312909747525783821 ) ) ;
#3527 = ORIENTED_EDGE ( 'NONE', *, *, #4675, .T. ) ;
#3528 = CARTESIAN_POINT ( 'NONE',  ( -39.38303923565386100, -44.70000000000000284, -1.486127417882099788 ) ) ;
#3529 = AXIS2_PLACEMENT_3D ( 'NONE', #2975, #4460, #3799 ) ;
#3530 = CARTESIAN_POINT ( 'NONE',  ( 4.999999999999998224, -44.99999999999997158, -98.49999999781503845 ) ) ;
#3531 = CARTESIAN_POINT ( 'NONE',  ( -2.071067811865475061, -39.99999999999997158, -98.24999999781505267 ) ) ;
#3532 = CARTESIAN_POINT ( 'NONE',  ( 3.535533905932737309, -48.53553390593270933, -98.59999999781504698 ) ) ;
#3533 = CARTESIAN_POINT ( 'NONE',  ( 4.999999999999998224, -44.99999999999997158, -97.69999999781505551 ) ) ;
#3534 = CARTESIAN_POINT ( 'NONE',  ( -4.566987299999998307, -43.10829192115428299, -97.69999999890751496 ) ) ;
#3535 = CARTESIAN_POINT ( 'NONE',  ( -36.35910488754074521, -43.25140427513058228, 6.280328284105565650 ) ) ;
#3536 = AXIS2_PLACEMENT_3D ( 'NONE', #4910, #191, #6314 ) ;
#3537 = CARTESIAN_POINT ( 'NONE',  ( -4.999999999999998224, -44.99999999999997158, -95.00000000000000000 ) ) ;
#3538 = PRODUCT_DEFINITION_CONTEXT ( 'detailed design', #7684, 'design' ) ;
#3539 = CARTESIAN_POINT ( 'NONE',  ( 4.566987300000000083, -46.89170807884565306, -96.49999999890752633 ) ) ;
#3540 = CARTESIAN_POINT ( 'NONE',  ( -25.94249218456686279, -46.65000000000001279, 7.963307464738194952 ) ) ;
#3541 = DIRECTION ( 'NONE',  ( 0.000000000000000000, 0.000000000000000000, 1.000000000000000000 ) ) ;
#3542 = EDGE_CURVE ( 'NONE', #6167, #2617, #6838, .T. ) ;
#3543 = DIRECTION ( 'NONE',  ( -0.000000000000000000, -0.000000000000000000, -1.000000000000000000 ) ) ;
#3544 = CARTESIAN_POINT ( 'NONE',  ( -28.60187809025093841, -42.44999999999999574, -8.827394325379140483 ) ) ;
#3545 = CARTESIAN_POINT ( 'NONE',  ( 27.34989276402963299, -40.75696118185767602, 12.21663313815757590 ) ) ;
#3546 = CYLINDRICAL_SURFACE ( 'NONE', #4500, 2.149999999999985256 ) ;
#3547 = CARTESIAN_POINT ( 'NONE',  ( -39.85719736222883824, -48.54859572486944330, 1.617624508639602388 ) ) ;
#3548 = DIRECTION ( 'NONE',  ( -0.000000000000000000, -0.000000000000000000, 1.000000000000000000 ) ) ;
#3549 = SURFACE_STYLE_USAGE ( .BOTH. , #233 ) ;
#3550 = ORIENTED_EDGE ( 'NONE', *, *, #3019, .T. ) ;
#3551 = DIRECTION ( 'NONE',  ( -0.000000000000000000, 1.000000000000000000, -0.000000000000000000 ) ) ;
#3552 = VERTEX_POINT ( 'NONE', #7639 ) ;
#3553 = CARTESIAN_POINT ( 'NONE',  ( -25.89286002894218086, -38.64859572486943762, 7.938018618334153231 ) ) ;
#3554 = CARTESIAN_POINT ( 'NONE',  ( -34.53486167607238144, -30.15000000000000213, -8.900167166472096270 ) ) ;
#3555 = CARTESIAN_POINT ( 'NONE',  ( -22.06198138166579170, -30.35140427513058015, 4.107139971057695682 ) ) ;
#3556 = AXIS2_PLACEMENT_3D ( 'NONE', #4549, #7859, #7368 ) ;
#3557 = ADVANCED_FACE ( 'NONE', ( #4341 ), #932, .F. ) ;
#3558 = ORIENTED_EDGE ( 'NONE', *, *, #2044, .T. ) ;
#3559 = CARTESIAN_POINT ( 'NONE',  ( -1.891708078845683039, -40.43301269999998482, -95.39999999890753202 ) ) ;
#3560 = DIRECTION ( 'NONE',  ( -1.000000000000000000, -0.000000000000000000, -0.000000000000000000 ) ) ;
#3561 = CIRCLE ( 'NONE', #8484, 2.149999999999985256 ) ;
#3562 = CARTESIAN_POINT ( 'NONE',  ( -33.05528180196482424, -41.02872310104125830, 12.12402686769023852 ) ) ;
#3563 = CARTESIAN_POINT ( 'NONE',  ( 3.229347689422839895, -41.77065231057713390, -98.94999999890752918 ) ) ;
#3564 = CYLINDRICAL_SURFACE ( 'NONE', #8627, 12.00000000000004263 ) ;
#3565 = LINE ( 'NONE', #5623, #6139 ) ;
#3566 = EDGE_LOOP ( 'NONE', ( #6019, #2855 ) ) ;
#3567 = CARTESIAN_POINT ( 'NONE',  ( -25.94249218456686279, -49.64999999999999147, 7.963307464738195840 ) ) ;
#3568 = CARTESIAN_POINT ( 'NONE',  ( -25.68709025247441602, -39.60000000000000853, -8.464561979789547053 ) ) ;
#3569 = CIRCLE ( 'NONE', #5780, 10.00000000000000178 ) ;
#3570 = AXIS2_PLACEMENT_3D ( 'NONE', #3087, #5765, #5851 ) ;
#3571 = EDGE_LOOP ( 'NONE', ( #6107, #236, #6486 ) ) ;
#3572 = CARTESIAN_POINT ( 'NONE',  ( -20.61696076434619584, -46.20000000000000284, 1.486127417882100676 ) ) ;
#3573 = CARTESIAN_POINT ( 'NONE',  ( -30.00000000000000000, -49.99999999999997158, 0.000000000000000000 ) ) ;
#3574 = CYLINDRICAL_SURFACE ( 'NONE', #7398, 1.649999999999998579 ) ;
#3575 = CARTESIAN_POINT ( 'NONE',  ( 2.071067811865477282, -49.99999999999996447, -100.2499999978150669 ) ) ;
#3576 = CARTESIAN_POINT ( 'NONE',  ( -21.09983283352784156, -49.35000000000000853, 4.534861676072186043 ) ) ;
#3577 = CARTESIAN_POINT ( 'NONE',  ( -4.566987299999998307, -43.10829192115428299, -98.49999999890752633 ) ) ;
#3578 = EDGE_LOOP ( 'NONE', ( #4886, #3735, #7957 ) ) ;
#3579 = CIRCLE ( 'NONE', #2315, 3.299999999999999822 ) ;
#3580 = CARTESIAN_POINT ( 'NONE',  ( -28.54686042191934092, -47.45140427513057091, -8.818680382772479120 ) ) ;
#3581 = CARTESIAN_POINT ( 'NONE',  ( -2.071067811865475505, -49.99999999999996447, -98.84300000002188824 ) ) ;
#3582 = FACE_OUTER_BOUND ( 'NONE', #5975, .T. ) ;
#3583 = CARTESIAN_POINT ( 'NONE',  ( -25.94249218456686279, -49.64999999999999858, 7.963307464738194952 ) ) ;
#3584 = CARTESIAN_POINT ( 'NONE',  ( -30.00000000000000000, -40.00000000000002132, 12.49999999999998046 ) ) ;
#3585 = AXIS2_PLACEMENT_3D ( 'NONE', #1660, #7031, #4475 ) ;
#3586 = APPLICATION_PROTOCOL_DEFINITION ( 'draft international standard', 'automotive_design', 1998, #1202 ) ;
#3587 = FILL_AREA_STYLE_COLOUR ( '', #5729 ) ;
#3588 = CARTESIAN_POINT ( 'NONE',  ( -31.39812190974910422, -40.95000000000000995, 8.827394325379140483 ) ) ;
#3589 = CARTESIAN_POINT ( 'NONE',  ( 25.66790131137006625, -42.48249851487847906, 11.72687238757475114 ) ) ;
#3590 = ADVANCED_FACE ( 'NONE', ( #7594, #4914 ), #852, .F. ) ;
#3591 = FACE_OUTER_BOUND ( 'NONE', #159, .T. ) ;
#3592 = CARTESIAN_POINT ( 'NONE',  ( -20.61696076434619584, -31.20000000000000639, 1.486127417882100676 ) ) ;
#3593 = CARTESIAN_POINT ( 'NONE',  ( 4.999999999999998224, -44.99999999999997158, -97.79999999999999716 ) ) ;
#3594 = LINE ( 'NONE', #6098, #3719 ) ;
#3595 = ORIENTED_EDGE ( 'NONE', *, *, #2699, .F. ) ;
#3596 = DIRECTION ( 'NONE',  ( -0.000000000000000000, -0.000000000000000000, 1.000000000000000000 ) ) ;
#3597 = ORIENTED_EDGE ( 'NONE', *, *, #441, .T. ) ;
#3598 = CARTESIAN_POINT ( 'NONE',  ( -26.18828373723858149, -40.59859572486944757, -7.597606577763319713 ) ) ;
#3599 = CARTESIAN_POINT ( 'NONE',  ( -28.51387258211773812, -31.80000000000000782, 9.383039235653802379 ) ) ;
#3600 = CARTESIAN_POINT ( 'NONE',  ( -25.51477047955235378, -48.65140427513057375, 8.925456012876139766 ) ) ;
#3601 = CARTESIAN_POINT ( 'NONE',  ( 1.891708078845682595, -40.43301269999998482, -97.09999999890753486 ) ) ;
#3602 = CARTESIAN_POINT ( 'NONE',  ( -30.00000000000000000, -40.00000000000002132, 12.49999999999998046 ) ) ;
#3603 = CARTESIAN_POINT ( 'NONE',  ( -4.566987299999998307, -44.99999999999997158, -97.84999999890752065 ) ) ;
#3604 = DIRECTION ( 'NONE',  ( -0.000000000000000000, -0.000000000000000000, -1.000000000000000000 ) ) ;
#3605 = AXIS2_PLACEMENT_3D ( 'NONE', #4334, #511, #7106 ) ;
#3606 = CARTESIAN_POINT ( 'NONE',  ( 2.071067811865477282, -49.99999999999997158, -96.24999999781505267 ) ) ;
#3607 = ORIENTED_EDGE ( 'NONE', *, *, #2863, .F. ) ;
#3608 = CARTESIAN_POINT ( 'NONE',  ( -37.54950433343896776, -42.39859572486944472, 3.906122232810848249 ) ) ;
#3609 = CARTESIAN_POINT ( 'NONE',  ( -38.46456197978948666, -44.40000000000000568, 4.312909747525784709 ) ) ;
#3610 = EDGE_LOOP ( 'NONE', ( #6790, #5894, #4783 ) ) ;
#3611 = CIRCLE ( 'NONE', #5858, 12.49999999999998757 ) ;
#3612 = CARTESIAN_POINT ( 'NONE',  ( -39.86591130483550671, -47.54999999999999716, 1.562606840307984468 ) ) ;
#3613 = CARTESIAN_POINT ( 'NONE',  ( -4.999999999999997335, -47.07106781186546129, -98.84999999781503277 ) ) ;
#3614 = FACE_OUTER_BOUND ( 'NONE', #6342, .T. ) ;
#3615 = ADVANCED_FACE ( 'NONE', ( #6888 ), #429, .F. ) ;
#3616 = CARTESIAN_POINT ( 'NONE',  ( -3.061616997868382155E-16, -39.99999999999997158, -98.29999999781504982 ) ) ;
#3617 = CARTESIAN_POINT ( 'NONE',  ( 42.00000000000000711, 48.00000000000002842, 21.99999999999992184 ) ) ;
#3618 = CARTESIAN_POINT ( 'NONE',  ( -4.566987299999998307, -44.99999999999997158, -100.0499999989075235 ) ) ;
#3619 = VERTEX_POINT ( 'NONE', #7687 ) ;
#3620 = CARTESIAN_POINT ( 'NONE',  ( -38.39535089505872634, -32.70000000000000995, -1.329692952841885267 ) ) ;
#3621 = CARTESIAN_POINT ( 'NONE',  ( 1.932551333443697450, -39.99999999999997158, -100.0396559164136931 ) ) ;
#3622 = CARTESIAN_POINT ( 'NONE',  ( 3.229347689422841228, -48.22934768942280925, -95.74999999890752633 ) ) ;
#3623 = CARTESIAN_POINT ( 'NONE',  ( -3.061616997868382155E-16, -39.99999999999997158, -97.49999999781503845 ) ) ;
#3624 = DIRECTION ( 'NONE',  ( -0.000000000000000000, -0.000000000000000000, -1.000000000000000000 ) ) ;
#3625 = VECTOR ( 'NONE', #3520, 1000.000000000000000 ) ;
#3626 = DIRECTION ( 'NONE',  ( 0.000000000000000000, -1.224646799147353207E-16, 1.000000000000000000 ) ) ;
#3627 = CIRCLE ( 'NONE', #1503, 11.99999999999983302 ) ;
#3628 = CARTESIAN_POINT ( 'NONE',  ( -33.85891924778610473, -35.10000000000000853, 7.573555455601171715 ) ) ;
#3629 = LINE ( 'NONE', #3222, #8256 ) ;
#3630 = CARTESIAN_POINT ( 'NONE',  ( -39.99999999999999289, 1.224646799147352862E-15, 80.00000000000002842 ) ) ;
#3631 = CARTESIAN_POINT ( 'NONE',  ( -28.43739315969223824, -36.45000000000000284, -9.865911304835512041 ) ) ;
#3632 = CARTESIAN_POINT ( 'NONE',  ( 0.6544984694978718265, -39.99999999999997868, -100.0000000000000142 ) ) ;
#3633 = CARTESIAN_POINT ( 'NONE',  ( -37.06321265474346660, -41.25000000000000711, 7.063212654743582952 ) ) ;
#3634 = AXIS2_PLACEMENT_3D ( 'NONE', #3099, #5242, #4420 ) ;
#3635 =( NAMED_UNIT ( * ) SI_UNIT ( $, .STERADIAN. ) SOLID_ANGLE_UNIT ( ) );
#3636 = ORIENTED_EDGE ( 'NONE', *, *, #689, .T. ) ;
#3637 = CARTESIAN_POINT ( 'NONE',  ( 42.00000000000000711, 48.00000000000002842, -21.99999999999992184 ) ) ;
#3638 = ORIENTED_EDGE ( 'NONE', *, *, #5580, .F. ) ;
#3639 = CARTESIAN_POINT ( 'NONE',  ( -22.01140368885771892, -38.34859572486944046, 4.007875659808335378 ) ) ;
#3640 = CARTESIAN_POINT ( 'NONE',  ( -21.55948914237271907, -49.89859572486943762, -4.360112732550413206 ) ) ;
#3641 = CARTESIAN_POINT ( 'NONE',  ( -28.72263195913613387, -30.80140427513057233, 8.403638346957361449 ) ) ;
#3642 = ADVANCED_FACE ( 'NONE', ( #2938 ), #7850, .F. ) ;
#3643 = CARTESIAN_POINT ( 'NONE',  ( 4.566987299999998307, -44.99999999999997158, -96.44999999890752918 ) ) ;
#3644 = DIRECTION ( 'NONE',  ( -0.000000000000000000, 1.000000000000000000, -0.000000000000000000 ) ) ;
#3645 = PRODUCT_DEFINITION_SHAPE ( 'NONE', 'NONE',  #8729 ) ;
#3646 = CARTESIAN_POINT ( 'NONE',  ( 4.566987300000000083, -46.89170807884565306, -98.29999999890752349 ) ) ;
#3647 = CYLINDRICAL_SURFACE ( 'NONE', #3024, 1.000000000000000888 ) ;
#3648 = CARTESIAN_POINT ( 'NONE',  ( 3.229347689422839895, -41.77065231057713390, -95.74999999890751212 ) ) ;
#3649 = CARTESIAN_POINT ( 'NONE',  ( -33.35889894354067309, -8.999999999999998224, 125.0000000000000000 ) ) ;
#3650 = ORIENTED_EDGE ( 'NONE', *, *, #5202, .F. ) ;
#3651 = ADVANCED_FACE ( 'NONE', ( #7021 ), #4957, .F. ) ;
#3652 = CARTESIAN_POINT ( 'NONE',  ( -26.18828373723858149, -43.59859572486944046, -7.597606577763319713 ) ) ;
#3653 = CARTESIAN_POINT ( 'NONE',  ( -31.56260684030781505, -46.94999999999998863, 9.865911304835510265 ) ) ;
#3654 = ORIENTED_EDGE ( 'NONE', *, *, #5197, .T. ) ;
#3655 = CARTESIAN_POINT ( 'NONE',  ( -20.62524821624488069, -30.20140427513057446, 1.538452329860250378 ) ) ;
#3656 = CARTESIAN_POINT ( 'NONE',  ( -36.71751442127229836, -30.00000000000000711, -6.717514421272142044 ) ) ;
#3657 = CARTESIAN_POINT ( 'NONE',  ( 42.00000000000000711, 60.00000000000002842, -21.99999999999992184 ) ) ;
#3658 = CARTESIAN_POINT ( 'NONE',  ( -4.999999999999998224, -42.92893218813448897, -98.14999999781504414 ) ) ;
#3659 = EDGE_CURVE ( 'NONE', #6288, #6070, #6934, .T. ) ;
#3660 = CARTESIAN_POINT ( 'NONE',  ( -41.99999999999996447, 48.00000000000002842, -20.35000000000000142 ) ) ;
#3661 = CARTESIAN_POINT ( 'NONE',  ( -3.535533905932735532, -48.53553390593270933, -95.70000000000000284 ) ) ;
#3662 = ORIENTED_EDGE ( 'NONE', *, *, #2998, .F. ) ;
#3663 = CARTESIAN_POINT ( 'NONE',  ( -21.17260567462091458, -31.05000000000000782, -1.398121909749242331 ) ) ;
#3664 = EDGE_CURVE ( 'NONE', #7971, #3431, #2634, .T. ) ;
#3665 = CARTESIAN_POINT ( 'NONE',  ( -2.071067811865475505, -49.99999999999996447, -99.64300000002187119 ) ) ;
#3666 = CARTESIAN_POINT ( 'NONE',  ( -4.566987299999998307, -43.10829192115428299, -95.29999999890750928 ) ) ;
#3667 = CARTESIAN_POINT ( 'NONE',  ( 2.071067811865477282, -49.99999999999996447, -97.84999999781504698 ) ) ;
#3668 = AXIS2_PLACEMENT_3D ( 'NONE', #4561, #991, #3165 ) ;
#3669 = CARTESIAN_POINT ( 'NONE',  ( -30.00000000000002487, 0.000000000000000000, -44.00000000000000000 ) ) ;
#3670 = CARTESIAN_POINT ( 'NONE',  ( -36.01040764008574513, -42.00000000000000711, -6.010407640085605685 ) ) ;
#3671 = PRODUCT ( 'position indicator', 'position indicator', '', ( #5510 ) ) ;
#3672 = FACE_OUTER_BOUND ( 'NONE', #7638, .T. ) ;
#3673 = CARTESIAN_POINT ( 'NONE',  ( -34.05750781543319050, -30.15000000000000568, -7.963307464738194952 ) ) ;
#3674 = CARTESIAN_POINT ( 'NONE',  ( -22.93678734525658314, -30.75000000000000000, -7.063212654743582952 ) ) ;
#3675 = LINE ( 'NONE', #7147, #4371 ) ;
#3676 = VECTOR ( 'NONE', #8345, 1000.000000000000000 ) ;
#3677 = CARTESIAN_POINT ( 'NONE',  ( -25.46513832392766119, -43.64999999999999858, 8.900167166472096270 ) ) ;
#3678 = ORIENTED_EDGE ( 'NONE', *, *, #6870, .F. ) ;
#3679 = ADVANCED_FACE ( 'NONE', ( #1815 ), #5564, .F. ) ;
#3680 = VERTEX_POINT ( 'NONE', #195 ) ;
#3681 = CARTESIAN_POINT ( 'NONE',  ( -34.10713997105786888, -37.14859572486943762, -7.938018618334151455 ) ) ;
#3682 = PRODUCT_RELATED_PRODUCT_CATEGORY ( 'part', '', ( #288 ) ) ;
#3683 = CARTESIAN_POINT ( 'NONE',  ( -23.24502507771338600, -50.49859572486944614, 6.680053920257780220 ) ) ;
#3684 = CARTESIAN_POINT ( 'NONE',  ( -22.89739904353894318, -47.75140427513058938, -7.023824353025938549 ) ) ;
#3685 = MECHANICAL_DESIGN_GEOMETRIC_PRESENTATION_REPRESENTATION (  '', ( #5089 ), #4810 ) ;
#3686 = CARTESIAN_POINT ( 'NONE',  ( -2.796473189345805913E-16, -40.43301269999997061, -100.2499999989075263 ) ) ;
#3687 = UNCERTAINTY_MEASURE_WITH_UNIT (LENGTH_MEASURE( 1.000000000000000082E-05 ), #7291, 'distance_accuracy_value', 'NONE');
#3688 = DIRECTION ( 'NONE',  ( 1.000000000000000000, 0.000000000000000000, 0.000000000000000000 ) ) ;
#3689 = CARTESIAN_POINT ( 'NONE',  ( -3.229347689422839451, -48.22934768942280925, -100.1499999989075178 ) ) ;
#3690 = CARTESIAN_POINT ( 'NONE',  ( 30.00000000000000000, -49.99999999999997158, -1.102182119232617753E-14 ) ) ;
#3691 = CARTESIAN_POINT ( 'NONE',  ( 4.566987299999998307, -43.10829192115428299, -98.19999999890751496 ) ) ;
#3692 = DIRECTION ( 'NONE',  ( 1.000000000000000000, 0.000000000000000000, 0.000000000000000000 ) ) ;
#3693 = ORIENTED_EDGE ( 'NONE', *, *, #5860, .F. ) ;
#3694 = CARTESIAN_POINT ( 'NONE',  ( -36.04786814110010340, -42.99859572486943904, -5.972947139071243861 ) ) ;
#3695 = CARTESIAN_POINT ( 'NONE',  ( -38.90016716647221529, -41.84999999999999432, -4.534861676072185155 ) ) ;
#3696 = VECTOR ( 'NONE', #2426, 1000.000000000000000 ) ;
#3697 = ORIENTED_EDGE ( 'NONE', *, *, #4497, .T. ) ;
#3698 = CARTESIAN_POINT ( 'NONE',  ( -21.51138689804841420, -38.90140427513058086, -4.265706762501151772 ) ) ;
#3699 = DIRECTION ( 'NONE',  ( -1.000000000000000000, -0.000000000000000000, -0.000000000000000000 ) ) ;
#3700 = DIRECTION ( 'NONE',  ( 1.000000000000000000, 0.000000000000000000, 0.000000000000000000 ) ) ;
#3701 = DIRECTION ( 'NONE',  ( -0.000000000000000000, -0.000000000000000000, 1.000000000000000000 ) ) ;
#3702 = DIRECTION ( 'NONE',  ( -0.000000000000000000, -0.000000000000000000, -1.000000000000000000 ) ) ;
#3703 = CARTESIAN_POINT ( 'NONE',  ( 2.071067811865474173, -39.99999999999997158, -95.25000000000000000 ) ) ;
#3704 = EDGE_LOOP ( 'NONE', ( #6202, #7305, #8372, #5769 ) ) ;
#3705 = ADVANCED_BREP_SHAPE_REPRESENTATION ( '', ( #8634, #2554 ), #564 ) ;
#3706 = CARTESIAN_POINT ( 'NONE',  ( -38.82739432537914581, -35.55000000000001137, 1.398121909749243441 ) ) ;
#3707 = CIRCLE ( 'NONE', #4828, 0.5000000000000001110 ) ;
#3708 = ORIENTED_EDGE ( 'NONE', *, *, #4588, .F. ) ;
#3709 = CARTESIAN_POINT ( 'NONE',  ( -4.566987299999998307, -43.10829192115428299, -96.09999999890752065 ) ) ;
#3710 = CARTESIAN_POINT ( 'NONE',  ( -37.57355545560112375, -50.40000000000000568, 3.858919247786223305 ) ) ;
#3711 = CARTESIAN_POINT ( 'NONE',  ( -25.64110105645932336, -7.999999999999996447, 125.0000000000000000 ) ) ;
#3712 = CARTESIAN_POINT ( 'NONE',  ( 30.00000000000000000, 60.00000000000002842, -1.102182119232617753E-14 ) ) ;
#3713 = CARTESIAN_POINT ( 'NONE',  ( -28.67030704715798350, -43.80000000000000426, 8.395350895058669494 ) ) ;
#3714 = FACE_OUTER_BOUND ( 'NONE', #1856, .T. ) ;
#3715 = CARTESIAN_POINT ( 'NONE',  ( 8.389419568037416259E-16, -49.56698729999997255, -96.04999999890752349 ) ) ;
#3716 = ADVANCED_FACE ( 'NONE', ( #5612 ), #8271, .T. ) ;
#3717 = CYLINDRICAL_SURFACE ( 'NONE', #8169, 2.149999999999985256 ) ;
#3718 = CARTESIAN_POINT ( 'NONE',  ( -39.86591130483550671, -38.54999999999999716, 1.562606840307984468 ) ) ;
#3719 = VECTOR ( 'NONE', #2847, 1000.000000000000000 ) ;
#3720 = FACE_OUTER_BOUND ( 'NONE', #200, .T. ) ;
#3721 = CARTESIAN_POINT ( 'NONE',  ( -21.53543802021056663, -39.90000000000000568, -4.312909747525783821 ) ) ;
#3722 = EDGE_LOOP ( 'NONE', ( #3335, #1556, #6761, #7430 ) ) ;
#3723 = ORIENTED_EDGE ( 'NONE', *, *, #8589, .F. ) ;
#3724 = CARTESIAN_POINT ( 'NONE',  ( -23.95213185889994989, -44.49859572486944614, 5.972947139071243861 ) ) ;
#3725 = CARTESIAN_POINT ( 'NONE',  ( -38.92545601287626056, -51.84859572486944757, -4.485229520447501450 ) ) ;
#3726 = CARTESIAN_POINT ( 'NONE',  ( -38.48861310195163554, -49.40140427513058086, 4.265706762501153548 ) ) ;
#3727 =( BOUNDED_CURVE ( )  B_SPLINE_CURVE ( 2, ( #472, #4544, #7938, #4376, #4499, #5198, #5121, #354, #7230 ),
 .UNSPECIFIED., .F., .T. ) 
 B_SPLINE_CURVE_WITH_KNOTS ( ( 3, 2, 2, 2, 3 ),
 ( 0.2142857142857142738, 0.2321428571428571508, 0.2500000000000000000, 0.2678571428571428492, 0.2857142857142856984 ),
 .UNSPECIFIED. ) 
 CURVE ( )  GEOMETRIC_REPRESENTATION_ITEM ( )  RATIONAL_B_SPLINE_CURVE ( ( 1.000000000000000000, 0.9238795325112867385, 1.000000000000000000, 0.9238795325112867385, 1.000000000000000000, 0.9238795325112867385, 1.000000000000000000, 0.9238795325112867385, 1.000000000000000000 ) ) 
 REPRESENTATION_ITEM ( '' )  );
#3728 = CARTESIAN_POINT ( 'NONE',  ( -3.229347689422840784, -41.77065231057713390, -98.54999999890752349 ) ) ;
#3729 = CARTESIAN_POINT ( 'NONE',  ( 25.12952813221809123, -46.14268964625811265, 11.51215629180720512 ) ) ;
#3730 = CARTESIAN_POINT ( 'NONE',  ( -34.31290974752564438, -38.10000000000000853, 8.464561979789547053 ) ) ;
#3731 = DIRECTION ( 'NONE',  ( -0.7061138087190628188, 0.05297714858780449426, 0.7061138087190792501 ) ) ;
#3732 = CYLINDRICAL_SURFACE ( 'NONE', #7375, 2.099999999999997868 ) ;
#3733 = CARTESIAN_POINT ( 'NONE',  ( -3.229347689422840784, -41.77065231057713390, -97.94999999890751496 ) ) ;
#3734 = LINE ( 'NONE', #1662, #3960 ) ;
#3735 = ORIENTED_EDGE ( 'NONE', *, *, #6983, .T. ) ;
#3736 = CARTESIAN_POINT ( 'NONE',  ( -21.59636165304264921, -41.19859572486944188, 1.277368040863740228 ) ) ;
#3737 = CARTESIAN_POINT ( 'NONE',  ( -31.48612741788231517, -48.30000000000001137, -9.383039235653804155 ) ) ;
#3738 = EDGE_LOOP ( 'NONE', ( #827, #4111 ) ) ;
#3739 = CARTESIAN_POINT ( 'NONE',  ( -34.48522952044771017, -35.15140427513058086, -8.925456012876139766 ) ) ;
#3740 = CARTESIAN_POINT ( 'NONE',  ( 2.000000000000000000, 0.8865213383406683745, -1.535500000000000753 ) ) ;
#3741 = CARTESIAN_POINT ( 'NONE',  ( -33.35889894354067309, 9.000000000000001776, 124.0000000000000000 ) ) ;
#3742 = CARTESIAN_POINT ( 'NONE',  ( 4.999999999999998224, -44.99999999999997158, -97.69999999781505551 ) ) ;
#3743 = DIRECTION ( 'NONE',  ( 0.000000000000000000, 0.000000000000000000, 1.000000000000000000 ) ) ;
#3744 = CARTESIAN_POINT ( 'NONE',  ( -4.999999999999997335, -47.07106781186546129, -96.54999999999999716 ) ) ;
#3745 = EDGE_LOOP ( 'NONE', ( #2473, #456, #1844, #7110, #3934 ) ) ;
#3746 = PRODUCT_DEFINITION_SHAPE ( 'NONE', 'NONE',  #8721 ) ;
#3747 = CARTESIAN_POINT ( 'NONE',  ( -23.98959235991431171, -37.50000000000000711, 6.010407640085604797 ) ) ;
#3748 = ORIENTED_EDGE ( 'NONE', *, *, #4949, .F. ) ;
#3749 = EDGE_CURVE ( 'NONE', #1695, #5699, #5282, .T. ) ;
#3750 = CARTESIAN_POINT ( 'NONE',  ( -4.999999999999998224, -42.92893218813448897, -96.64999999999999147 ) ) ;
#3751 = CARTESIAN_POINT ( 'NONE',  ( -4.999999999999997335, -47.07106781186546129, -98.04999999781504982 ) ) ;
#3752 = CARTESIAN_POINT ( 'NONE',  ( 30.00000000000000000, -49.99999999999997158, -1.102182119232617753E-14 ) ) ;
#3753 = VECTOR ( 'NONE', #6927, 1000.000000000000000 ) ;
#3754 = FACE_OUTER_BOUND ( 'NONE', #4231, .T. ) ;
#3755 = EDGE_CURVE ( 'NONE', #2964, #4084, #3462, .T. ) ;
#3756 = DIRECTION ( 'NONE',  ( 1.000000000000000000, 0.000000000000000000, 0.000000000000000000 ) ) ;
#3757 = CARTESIAN_POINT ( 'NONE',  ( 3.535533905932736420, -41.46446609406723383, -98.50000000000000000 ) ) ;
#3758 = CARTESIAN_POINT ( 'NONE',  ( -18.00000000000002132, 1.469576158976823947E-15, -29.65000000000000213 ) ) ;
#3759 = CARTESIAN_POINT ( 'NONE',  ( -34.35889894354067309, -9.999999999999998224, -25.00000000000000000 ) ) ;
#3760 = ADVANCED_FACE ( 'NONE', ( #759 ), #5859, .F. ) ;
#3761 = CARTESIAN_POINT ( 'NONE',  ( -28.43739315969223824, -42.45000000000000284, -9.865911304835512041 ) ) ;
#3762 = AXIS2_PLACEMENT_3D ( 'NONE', #2533, #7241, #5336 ) ;
#3763 =( LENGTH_UNIT ( ) NAMED_UNIT ( * ) SI_UNIT ( .MILLI., .METRE. ) );
#3764 = VERTEX_POINT ( 'NONE', #4202 ) ;
#3765 = CARTESIAN_POINT ( 'NONE',  ( -22.01140368885771892, -44.34859572486944046, 4.007875659808335378 ) ) ;
#3766 = COLOUR_RGB ( '', 0.09019608, 0.27058824, 0.51372549) ;
#3767 = CARTESIAN_POINT ( 'NONE',  ( -21.53543802021056663, -39.90000000000000568, -4.312909747525783821 ) ) ;
#3768 = CARTESIAN_POINT ( 'NONE',  ( -22.06198138166579170, -42.35140427513057659, 4.107139971057695682 ) ) ;
#3769 = EDGE_CURVE ( 'NONE', #3168, #6235, #4952, .T. ) ;
#3770 = CIRCLE ( 'NONE', #2228, 10.00000000000000178 ) ;
#3771 = CARTESIAN_POINT ( 'NONE',  ( 1.891708078845685481, -49.56698729999997255, -99.79999999890752349 ) ) ;
#3772 = CARTESIAN_POINT ( 'NONE',  ( 30.00000000000000000, -39.99999999999998579, 12.49999999999996625 ) ) ;
#3773 = CARTESIAN_POINT ( 'NONE',  ( -34.53486167607238144, -36.15000000000001279, -8.900167166472096270 ) ) ;
#3774 = DIRECTION ( 'NONE',  ( 0.000000000000000000, 0.4999999999999992784, -0.8660254037844390407 ) ) ;
#3775 = DIRECTION ( 'NONE',  ( -1.000000000000000000, -0.000000000000000000, -0.000000000000000000 ) ) ;
#3776 = CARTESIAN_POINT ( 'NONE',  ( -3.229347689422839451, -48.22934768942280925, -97.74999999890751212 ) ) ;
#3777 = EDGE_CURVE ( 'NONE', #2594, #724, #2068, .T. ) ;
#3778 = CARTESIAN_POINT ( 'NONE',  ( -36.01040764008574513, -51.00000000000000711, -6.010407640085605685 ) ) ;
#3779 = VERTEX_POINT ( 'NONE', #6839 ) ;
#3780 = CARTESIAN_POINT ( 'NONE',  ( -30.00000000000000000, -49.99999999999997158, 0.000000000000000000 ) ) ;
#3781 =( BOUNDED_CURVE ( )  B_SPLINE_CURVE ( 2, ( #502, #3132, #2511, #3214, #5811, #2466, #5898, #5148, #1133 ),
 .UNSPECIFIED., .F., .T. ) 
 B_SPLINE_CURVE_WITH_KNOTS ( ( 3, 2, 2, 2, 3 ),
 ( 0.3571428571428570953, 0.3750000000000000000, 0.3928571428571428492, 0.4107142857142856984, 0.4285714285714286031 ),
 .UNSPECIFIED. ) 
 CURVE ( )  GEOMETRIC_REPRESENTATION_ITEM ( )  RATIONAL_B_SPLINE_CURVE ( ( 1.000000000000000222, 0.9238795325112865164, 1.000000000000000000, 0.9238795325112867385, 1.000000000000000000, 0.9238795325112867385, 1.000000000000000000, 0.9238795325112865164, 1.000000000000000222 ) ) 
 REPRESENTATION_ITEM ( '' )  );
#3782 = CARTESIAN_POINT ( 'NONE',  ( -31.34310424141748896, -50.94859572486944899, 8.836108267985801845 ) ) ;
#3783 = CARTESIAN_POINT ( 'NONE',  ( -22.89739904353894318, -29.75140427513057517, -7.023824353025938549 ) ) ;
#3784 = ORIENTED_EDGE ( 'NONE', *, *, #2203, .T. ) ;
#3785 = CARTESIAN_POINT ( 'NONE',  ( -31.61762450863942320, -36.95140427513057801, 9.857197362228843573 ) ) ;
#3786 = FACE_OUTER_BOUND ( 'NONE', #1031, .T. ) ;
#3787 = CARTESIAN_POINT ( 'NONE',  ( -34.35889894354067309, 9.000000000000001776, -24.00000000000000000 ) ) ;
#3788 = CARTESIAN_POINT ( 'NONE',  ( 9.184850993605145972E-16, -49.99999999999997158, -95.60000000000000853 ) ) ;
#3789 = CARTESIAN_POINT ( 'NONE',  ( -30.00000000000002487, 0.000000000000000000, -28.65000000000000213 ) ) ;
#3790 = CARTESIAN_POINT ( 'NONE',  ( -2.071067811865475061, -39.99999999999997158, -96.75000000000001421 ) ) ;
#3791 = ORIENTED_EDGE ( 'NONE', *, *, #6970, .T. ) ;
#3792 = CARTESIAN_POINT ( 'NONE',  ( -22.42644454439892598, -30.90000000000000924, -3.858919247786222861 ) ) ;
#3793 = ORIENTED_EDGE ( 'NONE', *, *, #8340, .T. ) ;
#3794 = CARTESIAN_POINT ( 'NONE',  ( -2.071067811865475505, -49.99999999999996447, -97.25000000000000000 ) ) ;
#3795 = CARTESIAN_POINT ( 'NONE',  ( -2.740268896160362289, -40.77945301579084969, -99.99896619294457878 ) ) ;
#3796 = DIRECTION ( 'NONE',  ( -0.000000000000000000, -0.000000000000000000, -1.000000000000000000 ) ) ;
#3797 = PLANE ( 'NONE',  #2090 ) ;
#3798 = VECTOR ( 'NONE', #273, 1000.000000000000000 ) ;
#3799 = DIRECTION ( 'NONE',  ( 0.000000000000000000, 0.000000000000000000, 1.000000000000000000 ) ) ;
#3800 = ADVANCED_FACE ( 'NONE', ( #1509 ), #4887, .F. ) ;
#3801 = CYLINDRICAL_SURFACE ( 'NONE', #7714, 4.999999999999998224 ) ;
#3802 = CARTESIAN_POINT ( 'NONE',  ( -38.46456197978948666, -50.40000000000000568, 4.312909747525784709 ) ) ;
#3803 = B_SPLINE_CURVE_WITH_KNOTS ( 'NONE', 3,
 ( #3226, #3969, #5863, #558, #3795, #6562, #1858, #8682, #4456, #3183, #3927, #514, #6647, #6602, #8597, #3269, #1814, #5118, #603, #5950, #7810, #5908, #6475, #8643, #2609, #5157, #6517, #7142, #5277, #7225, #427, #8555, #2562, #2519, #3143, #5240, #7183, #2475, #7934, #3317, #7982, #1943, #1269, #1103, #5195, #5823 ),
 .UNSPECIFIED., .F., .F.,
 ( 4, 2, 2, 2, 2, 2, 2, 2, 2, 2, 2, 2, 2, 2, 2, 2, 2, 2, 2, 2, 2, 2, 4 ),
 ( 0.000000000000000000, 0.06249999999999973632, 0.1249999999999994726, 0.1562499999999996114, 0.1874999999999997780, 0.2500000000000000555, 0.2812499999999998335, 0.3124999999999995559, 0.3749999999999990563, 0.4062499999999988343, 0.4374999999999986122, 0.4999999999999986677, 0.5624999999999987788, 0.5937499999999987788, 0.6249999999999988898, 0.6874999999999992228, 0.7187499999999993339, 0.7499999999999993339, 0.8124999999999995559, 0.8437499999999996669, 0.8749999999999997780, 0.9374999999999998890, 1.000000000000000000 ),
 .UNSPECIFIED. ) ;
#3804 = EDGE_LOOP ( 'NONE', ( #1112, #5230, #5308, #2910 ) ) ;
#3805 = CARTESIAN_POINT ( 'NONE',  ( -31.34310424141748896, -50.94859572486944899, 8.836108267985801845 ) ) ;
#3806 = CARTESIAN_POINT ( 'NONE',  ( -37.06321265474346660, -32.25000000000000711, 7.063212654743582952 ) ) ;
#3807 = CARTESIAN_POINT ( 'NONE',  ( -38.83610826798580717, -43.55140427513057944, 1.343104241417631073 ) ) ;
#3808 = AXIS2_PLACEMENT_3D ( 'NONE', #1245, #12, #2097 ) ;
#3809 = CARTESIAN_POINT ( 'NONE',  ( -26.64110105645932336, -8.999999999999998224, 125.0000000000000000 ) ) ;
#3810 = CARTESIAN_POINT ( 'NONE',  ( 25.17038609909130287, -46.30459253935128316, 11.52942094433410070 ) ) ;
#3811 = CARTESIAN_POINT ( 'NONE',  ( -22.97617564697422665, -34.74859572486943904, -7.102600956461224690 ) ) ;
#3812 = CARTESIAN_POINT ( 'NONE',  ( -25.46513832392765408, -34.64999999999998437, 8.900167166472096270 ) ) ;
#3813 = PRODUCT ( 'shock absorber', 'shock absorber', '', ( #2886 ) ) ;
#3814 = CARTESIAN_POINT ( 'NONE',  ( -3.229347689422840784, -41.77065231057713390, -99.54999999890752349 ) ) ;
#3815 = DIRECTION ( 'NONE',  ( 0.000000000000000000, 0.000000000000000000, -1.000000000000000000 ) ) ;
#3816 = CARTESIAN_POINT ( 'NONE',  ( 4.566987299999998307, -44.99999999999997158, -95.84999999890752065 ) ) ;
#3817 = ORIENTED_EDGE ( 'NONE', *, *, #7026, .F. ) ;
#3818 =( LENGTH_UNIT ( ) NAMED_UNIT ( * ) SI_UNIT ( .MILLI., .METRE. ) );
#3819 = CARTESIAN_POINT ( 'NONE',  ( -31.34310424141748896, -47.94859572486943478, 8.836108267985801845 ) ) ;
#3820 = CARTESIAN_POINT ( 'NONE',  ( -21.51138689804841420, -29.90140427513058796, -4.265706762501151772 ) ) ;
#3821 = COLOUR_RGB ( '', 0.66274510, 0.83137255, 0.94901961) ;
#3822 = ADVANCED_FACE ( 'NONE', ( #1422 ), #4117, .F. ) ;
#3823 = ORIENTED_EDGE ( 'NONE', *, *, #7586, .T. ) ;
#3824 = CARTESIAN_POINT ( 'NONE',  ( -31.61762450863942320, -33.95140427513058512, 9.857197362228843573 ) ) ;
#3825 = CARTESIAN_POINT ( 'NONE',  ( -41.99999999999996447, -22.00000000000000000, 60.00000000000002842 ) ) ;
#3826 = DIRECTION ( 'NONE',  ( -0.000000000000000000, -0.000000000000000000, -1.000000000000000000 ) ) ;
#3827 = FACE_OUTER_BOUND ( 'NONE', #4439, .T. ) ;
#3828 = COLOUR_RGB ( '', 0.40784314, 0.44705882, 0.49803922) ;
#3829 = DIRECTION ( 'NONE',  ( -0.000000000000000000, 1.000000000000000000, -0.000000000000000000 ) ) ;
#3830 = CARTESIAN_POINT ( 'NONE',  ( -3.061616997868382155E-16, -39.99999999999997158, -95.20000000000000284 ) ) ;
#3831 = ORIENTED_EDGE ( 'NONE', *, *, #5667, .T. ) ;
#3832 = CARTESIAN_POINT ( 'NONE',  ( -38.82739432537914581, -41.55000000000001137, 1.398121909749243441 ) ) ;
#3833 = ORIENTED_EDGE ( 'NONE', *, *, #701, .T. ) ;
#3834 = CARTESIAN_POINT ( 'NONE',  ( 3.535533905932737309, -48.53553390593270933, -96.29999999999999716 ) ) ;
#3835 = CARTESIAN_POINT ( 'NONE',  ( -44.14999999999995595, -22.00000000000000000, 80.00000000000002842 ) ) ;
#3836 = ADVANCED_FACE ( 'NONE', ( #6798 ), #3546, .F. ) ;
#3837 = CARTESIAN_POINT ( 'NONE',  ( -38.38706344316003793, -31.70140427513057091, -1.382017864820032083 ) ) ;
#3838 = CARTESIAN_POINT ( 'NONE',  ( -20.00000000000000355, 0.000000000000000000, 60.00000000000002842 ) ) ;
#3839 = AXIS2_PLACEMENT_3D ( 'NONE', #183, #2085, #5509 ) ;
#3840 = VECTOR ( 'NONE', #5977, 1000.000000000000000 ) ;
#3841 = CARTESIAN_POINT ( 'NONE',  ( 2.000000000000000000, -1.773042676681341634, 2.493664996716660198E-15 ) ) ;
#3842 = CARTESIAN_POINT ( 'NONE',  ( -37.96330746473829976, -32.85000000000000142, -4.057507815433013754 ) ) ;
#3843 = CYLINDRICAL_SURFACE ( 'NONE', #6860, 1.000000000000000888 ) ;
#3844 = FACE_OUTER_BOUND ( 'NONE', #150, .T. ) ;
#3845 = DIRECTION ( 'NONE',  ( -1.000000000000000000, 0.000000000000000000, 0.000000000000000000 ) ) ;
#3846 = STYLED_ITEM ( 'NONE', ( #5929 ), #3048 ) ;
#3847 = ORIENTED_EDGE ( 'NONE', *, *, #7026, .T. ) ;
#3848 = CARTESIAN_POINT ( 'NONE',  ( -22.01140368885771892, -47.34859572486942625, 4.007875659808335378 ) ) ;
#3849 = CARTESIAN_POINT ( 'NONE',  ( -34.31290974752564438, -38.10000000000000853, 8.464561979789547053 ) ) ;
#3850 = CARTESIAN_POINT ( 'NONE',  ( -37.59760657776328685, -37.40140427513058796, 3.811716262761598362 ) ) ;
#3851 = ADVANCED_FACE ( 'NONE', ( #102 ), #189, .T. ) ;
#3852 = AXIS2_PLACEMENT_3D ( 'NONE', #8618, #6668, #1164 ) ;
#3853 = CARTESIAN_POINT ( 'NONE',  ( 4.566987300000000083, -46.89170807884564596, -98.09999999890753486 ) ) ;
#3854 = UNCERTAINTY_MEASURE_WITH_UNIT (LENGTH_MEASURE( 1.000000000000000082E-05 ), #8044, 'distance_accuracy_value', 'NONE');
#3855 = FACE_OUTER_BOUND ( 'NONE', #2545, .T. ) ;
#3856 = CARTESIAN_POINT ( 'NONE',  ( -21.55948914237271907, -34.89859572486943762, -4.360112732550413206 ) ) ;
#3857 = CARTESIAN_POINT ( 'NONE',  ( -34.53486167607238144, -39.14999999999999147, -8.900167166472096270 ) ) ;
#3858 = DIRECTION ( 'NONE',  ( -0.000000000000000000, -0.000000000000000000, -1.000000000000000000 ) ) ;
#3859 = DIRECTION ( 'NONE',  ( -0.000000000000000000, 1.000000000000000000, -0.000000000000000000 ) ) ;
#3860 = CARTESIAN_POINT ( 'NONE',  ( 4.566987300000000083, -46.89170807884565306, -95.69999999890755760 ) ) ;
#3861 = CARTESIAN_POINT ( 'NONE',  ( 4.000000000000000000, 3.500000000000000000, 0.000000000000000000 ) ) ;
#3862 = EDGE_LOOP ( 'NONE', ( #5494, #7552, #4570, #75 ) ) ;
#3863 = DIRECTION ( 'NONE',  ( 1.000000000000000000, 0.000000000000000000, 0.000000000000000000 ) ) ;
#3864 = CARTESIAN_POINT ( 'NONE',  ( -22.45049566656107842, -49.89859572486943762, -3.906122232810846917 ) ) ;
#3865 = AXIS2_PLACEMENT_3D ( 'NONE', #45, #5417, #3541 ) ;
#3866 = CARTESIAN_POINT ( 'NONE',  ( -39.37475178375516549, -31.70140427513057091, -1.538452329860249712 ) ) ;
#3867 = ADVANCED_FACE ( 'NONE', ( #2890 ), #546, .T. ) ;
#3868 = EDGE_LOOP ( 'NONE', ( #8156, #5342 ) ) ;
#3869 = ORIENTED_EDGE ( 'NONE', *, *, #3181, .T. ) ;
#3870 = CARTESIAN_POINT ( 'NONE',  ( -38.48861310195163554, -37.40140427513058796, 4.265706762501153548 ) ) ;
#3871 = CARTESIAN_POINT ( 'NONE',  ( -34.67778767197271605, -46.77334385938317496, 11.59192968702633486 ) ) ;
#3872 = DIRECTION ( 'NONE',  ( 0.000000000000000000, 0.000000000000000000, 1.000000000000000000 ) ) ;
#3873 = CARTESIAN_POINT ( 'NONE',  ( -34.35889894354067309, -7.999999999999996447, 124.0000000000000000 ) ) ;
#3874 = CARTESIAN_POINT ( 'NONE',  ( 32.23131546658671454, -49.48665499171476512, 12.30309571437651428 ) ) ;
#3875 = DIRECTION ( 'NONE',  ( 1.000000000000000000, 0.000000000000000000, 0.000000000000000000 ) ) ;
#3876 = EDGE_LOOP ( 'NONE', ( #853, #123, #3386, #5247, #5128, #5637, #477, #4251 ) ) ;
#3877 = CARTESIAN_POINT ( 'NONE',  ( -23.68028341417693738, -42.75000000000001421, -6.319716585823198507 ) ) ;
#3878 = EDGE_CURVE ( 'NONE', #6156, #7382, #7545, .T. ) ;
#3879 = EDGE_LOOP ( 'NONE', ( #1694, #5102, #7425, #4482 ) ) ;
#3880 = CARTESIAN_POINT ( 'NONE',  ( -4.999999999999997335, -47.07106781186546129, -96.54999999999999716 ) ) ;
#3881 = CARTESIAN_POINT ( 'NONE',  ( -34.31290974752564438, -38.10000000000000853, 8.464561979789547053 ) ) ;
#3882 = DIRECTION ( 'NONE',  ( 1.000000000000000000, 0.000000000000000000, 0.000000000000000000 ) ) ;
#3883 = CARTESIAN_POINT ( 'NONE',  ( -34.00787565980851213, -29.15140427513058441, -7.988596311142238449 ) ) ;
#3884 = CARTESIAN_POINT ( 'NONE',  ( -3.061616997868382155E-16, -39.99999999999997158, -99.89999999781504414 ) ) ;
#3885 = AXIS2_PLACEMENT_3D ( 'NONE', #3011, #2879, #4988 ) ;
#3886 = CARTESIAN_POINT ( 'NONE',  ( -22.03669253526174998, -37.35000000000000853, 4.057507815433014642 ) ) ;
#3887 = CARTESIAN_POINT ( 'NONE',  ( 29.66573552397922242, -49.99999999999991473, 12.49999999999996803 ) ) ;
#3888 = VECTOR ( 'NONE', #4293, 1000.000000000000000 ) ;
#3889 = DIRECTION ( 'NONE',  ( -0.000000000000000000, -0.000000000000000000, 1.000000000000000000 ) ) ;
#3890 = DIRECTION ( 'NONE',  ( 1.000000000000000000, 0.000000000000000000, 0.000000000000000000 ) ) ;
#3891 = ORIENTED_EDGE ( 'NONE', *, *, #2526, .T. ) ;
#3892 = CARTESIAN_POINT ( 'NONE',  ( -28.61798213517984024, -47.79859572486944330, 8.387063443159973986 ) ) ;
#3893 = CARTESIAN_POINT ( 'NONE',  ( -21.09983283352784156, -37.35000000000000853, 4.534861676072186043 ) ) ;
#3894 = CARTESIAN_POINT ( 'NONE',  ( -35.97294713907137975, -44.00140427513057517, -6.047868141099968398 ) ) ;
#3895 = DIRECTION ( 'NONE',  ( -0.000000000000000000, -0.000000000000000000, -1.000000000000000000 ) ) ;
#3896 = CIRCLE ( 'NONE', #5291, 1.324999999999999734 ) ;
#3897 = CARTESIAN_POINT ( 'NONE',  ( -34.35889894354067309, -7.999999999999996447, -24.00000000000000000 ) ) ;
#3898 = CARTESIAN_POINT ( 'NONE',  ( -39.39132668755255651, -36.69859572486944188, -1.433802505903950308 ) ) ;
#3899 = CARTESIAN_POINT ( 'NONE',  ( -21.53543802021056663, -42.90000000000000568, -4.312909747525783821 ) ) ;
#3900 = EDGE_CURVE ( 'NONE', #5916, #2514, #4777, .T. ) ;
#3901 = CARTESIAN_POINT ( 'NONE',  ( -31.74999999999995737, 0.000000000000000000, 0.000000000000000000 ) ) ;
#3902 = FACE_OUTER_BOUND ( 'NONE', #8146, .T. ) ;
#3903 = CARTESIAN_POINT ( 'NONE',  ( 4.566987299999998307, -43.10829192115428299, -99.79999999890752349 ) ) ;
#3904 = EDGE_LOOP ( 'NONE', ( #8667, #2896, #5028, #8192 ) ) ;
#3905 = CARTESIAN_POINT ( 'NONE',  ( -30.00000000000000000, 0.000000000000000000, 60.00000000000002842 ) ) ;
#3906 = CARTESIAN_POINT ( 'NONE',  ( -26.18828373723858149, -46.59859572486944046, -7.597606577763319713 ) ) ;
#3907 = CARTESIAN_POINT ( 'NONE',  ( -25.63988726744978663, -29.60140427513057659, -8.440510857627391061 ) ) ;
#3908 = ADVANCED_FACE ( 'NONE', ( #3591, #2141 ), #8266, .T. ) ;
#3909 = AXIS2_PLACEMENT_3D ( 'NONE', #5281, #4066, #520 ) ;
#3910 = VERTEX_POINT ( 'NONE', #1551 ) ;
#3911 = ORIENTED_EDGE ( 'NONE', *, *, #778, .F. ) ;
#3912 = CARTESIAN_POINT ( 'NONE',  ( -21.12512167993187973, -42.35140427513057659, 4.584493831696868860 ) ) ;
#3913 = CARTESIAN_POINT ( 'NONE',  ( 0.000000000000000000, -0.8865213383406692627, 1.535500000000001641 ) ) ;
#3914 = CARTESIAN_POINT ( 'NONE',  ( -31.74999999999995737, 0.000000000000000000, 0.000000000000000000 ) ) ;
#3915 = CARTESIAN_POINT ( 'NONE',  ( -37.96330746473829976, -50.85000000000000142, -4.057507815433013754 ) ) ;
#3916 = PLANE ( 'NONE',  #315 ) ;
#3917 = DIRECTION ( 'NONE',  ( 1.000000000000000000, -0.000000000000000000, -0.000000000000000000 ) ) ;
#3918 = ADVANCED_FACE ( 'NONE', ( #4245 ), #229, .T. ) ;
#3919 = ORIENTED_EDGE ( 'NONE', *, *, #4770, .F. ) ;
#3920 = CARTESIAN_POINT ( 'NONE',  ( -28.60187809025093841, -45.45000000000000995, -8.827394325379140483 ) ) ;
#3921 = EDGE_CURVE ( 'NONE', #5699, #1695, #4793, .T. ) ;
#3922 = EDGE_LOOP ( 'NONE', ( #5655, #6762, #2528, #7963 ) ) ;
#3923 = CARTESIAN_POINT ( 'NONE',  ( -18.00000000000019185, 1.469576158976803042E-15, -40.35000000000000142 ) ) ;
#3924 = CARTESIAN_POINT ( 'NONE',  ( 5.000000000000000000, -47.07106781186545419, -99.45000000000000284 ) ) ;
#3925 = CARTESIAN_POINT ( 'NONE',  ( -28.43739315969223824, -48.44999999999999574, -9.865911304835512041 ) ) ;
#3926 = CARTESIAN_POINT ( 'NONE',  ( 4.566987300000000083, -46.89170807884565306, -99.69999999890752918 ) ) ;
#3927 = CARTESIAN_POINT ( 'NONE',  ( -4.794783009932419127, -43.47026749230783338, -99.99939984573538254 ) ) ;
#3928 = EDGE_CURVE ( 'NONE', #5629, #5205, #1466, .T. ) ;
#3929 = CARTESIAN_POINT ( 'NONE',  ( -23.64089511245930098, -35.75140427513057517, -6.280328284105564762 ) ) ;
#3930 = CARTESIAN_POINT ( 'NONE',  ( 3.535533905932737309, -48.53553390593270933, -96.29300000002184845 ) ) ;
#3931 = CARTESIAN_POINT ( 'NONE',  ( -21.17260567462091103, -37.05000000000000426, -1.398121909749241887 ) ) ;
#3932 = CARTESIAN_POINT ( 'NONE',  ( -41.99999999999996447, -22.00000000000000000, 80.00000000000002842 ) ) ;
#3933 = CARTESIAN_POINT ( 'NONE',  ( -30.00000000000002842, 52.67500000000002558, 0.000000000000000000 ) ) ;
#3934 = ORIENTED_EDGE ( 'NONE', *, *, #137, .T. ) ;
#3935 = CARTESIAN_POINT ( 'NONE',  ( 50.00000000000002842, -44.99999999999997158, -2.099999999999997868 ) ) ;
#3936 = CARTESIAN_POINT ( 'NONE',  ( -37.06321265474346660, -35.24999999999998579, 7.063212654743582952 ) ) ;
#3937 = CARTESIAN_POINT ( 'NONE',  ( -38.83610826798580717, -40.55140427513058654, 1.343104241417631073 ) ) ;
#3938 = CIRCLE ( 'NONE', #2824, 2.149999999999985256 ) ;
#3939 = DIRECTION ( 'NONE',  ( -0.000000000000000000, 1.000000000000000000, -0.000000000000000000 ) ) ;
#3940 = FACE_OUTER_BOUND ( 'NONE', #3425, .T. ) ;
#3941 = CARTESIAN_POINT ( 'NONE',  ( -39.85719736222883824, -39.54859572486944330, 1.617624508639602388 ) ) ;
#3942 = DIRECTION ( 'NONE',  ( 0.000000000000000000, 0.000000000000000000, 1.000000000000000000 ) ) ;
#3943 = ADVANCED_FACE ( 'NONE', ( #936 ), #3717, .F. ) ;
#3944 = CARTESIAN_POINT ( 'NONE',  ( 34.00000000000000000, 0.000000000000000000, 0.000000000000000000 ) ) ;
#3945 = CARTESIAN_POINT ( 'NONE',  ( -4.566987299999998307, -43.10829192115428299, -99.49999999890754054 ) ) ;
#3946 = VECTOR ( 'NONE', #5561, 1000.000000000000000 ) ;
#3947 = ORIENTED_EDGE ( 'NONE', *, *, #793, .T. ) ;
#3948 = CARTESIAN_POINT ( 'NONE',  ( -7.499999999999999112, -44.99999999999997158, -105.0000000000000142 ) ) ;
#3949 = CARTESIAN_POINT ( 'NONE',  ( -34.58449383169706692, -31.14859572486944828, -8.874878320068054549 ) ) ;
#3950 = CARTESIAN_POINT ( 'NONE',  ( -20.12537475255788522, -36.05140427513057944, -1.507589171976365439 ) ) ;
#3951 = EDGE_LOOP ( 'NONE', ( #7048, #1470, #1569, #4789, #4579 ) ) ;
#3952 = ORIENTED_EDGE ( 'NONE', *, *, #7252, .F. ) ;
#3953 = CARTESIAN_POINT ( 'NONE',  ( -34.36011273255026310, -49.10140427513058370, 8.440510857627391061 ) ) ;
#3954 = SURFACE_SIDE_STYLE ('',( #4086 ) ) ;
#3955 = DIRECTION ( 'NONE',  ( 0.000000000000000000, 0.000000000000000000, 1.000000000000000000 ) ) ;
#3956 = CARTESIAN_POINT ( 'NONE',  ( -2.071067811865475505, -49.99999999999996447, -100.3499999978150754 ) ) ;
#3957 = CARTESIAN_POINT ( 'NONE',  ( -4.999999999999998224, -44.99999999999997158, -95.00000000000000000 ) ) ;
#3958 = CARTESIAN_POINT ( 'NONE',  ( -4.999999999999997335, -47.07106781186546129, -99.75000000000001421 ) ) ;
#3959 = ORIENTED_EDGE ( 'NONE', *, *, #8077, .F. ) ;
#3960 = VECTOR ( 'NONE', #3080, 1000.000000000000000 ) ;
#3961 = CARTESIAN_POINT ( 'NONE',  ( -28.67030704715798350, -43.80000000000000426, 8.395350895058669494 ) ) ;
#3962 =( GEOMETRIC_REPRESENTATION_CONTEXT ( 3 ) GLOBAL_UNCERTAINTY_ASSIGNED_CONTEXT ( ( #8388 ) ) GLOBAL_UNIT_ASSIGNED_CONTEXT ( ( #4077, #149, #2186 ) ) REPRESENTATION_CONTEXT ( 'NONE', 'WORKASPACE' ) );
#3963 = EDGE_CURVE ( 'NONE', #5746, #1056, #3238, .T. ) ;
#3964 = DIRECTION ( 'NONE',  ( 0.000000000000000000, -0.4999999999999992784, 0.8660254037844389297 ) ) ;
#3965 = CARTESIAN_POINT ( 'NONE',  ( -3.229347689422839451, -48.22934768942280925, -98.54999999890752349 ) ) ;
#3966 = CARTESIAN_POINT ( 'NONE',  ( 3.535533905932737309, -48.53553390593270933, -96.19999999781504130 ) ) ;
#3967 = CARTESIAN_POINT ( 'NONE',  ( -28.43739315969223824, -39.45000000000000995, -9.865911304835512041 ) ) ;
#3968 = CARTESIAN_POINT ( 'NONE',  ( 8.389419568037416259E-16, -49.56698729999997255, -99.84999999890753486 ) ) ;
#3969 = CARTESIAN_POINT ( 'NONE',  ( -0.5580800036469334424, -39.99999999999998579, -100.0011100901508883 ) ) ;
#3970 = CARTESIAN_POINT ( 'NONE',  ( -28.54686042191934092, -35.45140427513057801, -8.818680382772479120 ) ) ;
#3971 = EDGE_CURVE ( 'NONE', #1249, #1795, #2993, .T. ) ;
#3972 = CARTESIAN_POINT ( 'NONE',  ( -3.535533905932736864, -41.46446609406723383, -96.69300000002185413 ) ) ;
#3973 = AXIS2_PLACEMENT_3D ( 'NONE', #5317, #2439, #7724 ) ;
#3974 = CARTESIAN_POINT ( 'NONE',  ( -38.39535089505872634, -32.70000000000000995, -1.329692952841885267 ) ) ;
#3975 = CARTESIAN_POINT ( 'NONE',  ( 33.61000000000001364, 2.449293598294707893E-16, -2.000000000000000888 ) ) ;
#3976 = DIRECTION ( 'NONE',  ( -0.000000000000000000, 0.000000000000000000, -1.000000000000000000 ) ) ;
#3977 = DIRECTION ( 'NONE',  ( 0.000000000000000000, 0.000000000000000000, -1.000000000000000000 ) ) ;
#3978 = ORIENTED_EDGE ( 'NONE', *, *, #486, .F. ) ;
#3979 = FACE_BOUND ( 'NONE', #5491, .T. ) ;
#3980 = CARTESIAN_POINT ( 'NONE',  ( -38.90016716647221529, -44.85000000000001563, -4.534861676072185155 ) ) ;
#3981 = AXIS2_PLACEMENT_3D ( 'NONE', #2428, #1767, #1849 ) ;
#3982 = CARTESIAN_POINT ( 'NONE',  ( -31.45313957808072303, -48.95140427513057091, 8.818680382772479120 ) ) ;
#3983 = CARTESIAN_POINT ( 'NONE',  ( -3.061616997868382155E-16, -39.99999999999997158, -96.79999999999999716 ) ) ;
#3984 = CARTESIAN_POINT ( 'NONE',  ( -41.99999999999996447, 60.00000000000002842, 23.64999999999999858 ) ) ;
#3985 = CARTESIAN_POINT ( 'NONE',  ( -34.26570676250101855, -39.09859572486944046, 8.488613101951703044 ) ) ;
#3986 = CARTESIAN_POINT ( 'NONE',  ( -20.00000000000002487, 0.000000000000000000, -28.65000000000000213 ) ) ;
#3987 = COLOUR_RGB ( '', 0.40784314, 0.44705882, 0.49803922) ;
#3988 = DIRECTION ( 'NONE',  ( 0.000000000000000000, 0.000000000000000000, 1.000000000000000000 ) ) ;
#3989 = CARTESIAN_POINT ( 'NONE',  ( -1.891708078845683039, -40.43301269999998482, -95.39999999890751781 ) ) ;
#3990 = FILL_AREA_STYLE ('',( #8575 ) ) ;
#3991 = ORIENTED_EDGE ( 'NONE', *, *, #3113, .F. ) ;
#3992 = DIRECTION ( 'NONE',  ( 0.000000000000000000, -0.000000000000000000, -1.000000000000000000 ) ) ;
#3993 = CARTESIAN_POINT ( 'NONE',  ( -21.17260567462091458, -46.05000000000001137, -1.398121909749242331 ) ) ;
#3994 = CARTESIAN_POINT ( 'NONE',  ( -31.53845232986046554, -40.29859572486944330, -9.374751783755117529 ) ) ;
#3995 = CARTESIAN_POINT ( 'NONE',  ( -28.56619749409589204, -36.80140427513057944, 9.391326687552490782 ) ) ;
#3996 = ORIENTED_EDGE ( 'NONE', *, *, #5318, .T. ) ;
#3997 = EDGE_LOOP ( 'NONE', ( #4220, #6405, #2644, #1979 ) ) ;
#3998 = CARTESIAN_POINT ( 'NONE',  ( -22.89739904353894318, -44.75140427513058228, -7.023824353025938549 ) ) ;
#3999 = FILL_AREA_STYLE ('',( #637 ) ) ;
#4000 = CARTESIAN_POINT ( 'NONE',  ( -41.99999999999985789, 0.000000000000000000, -40.35000000000000142 ) ) ;
#4001 = CARTESIAN_POINT ( 'NONE',  ( -4.566987299999998307, -43.10829192115428299, -95.49999999890754054 ) ) ;
#4002 = CARTESIAN_POINT ( 'NONE',  ( 34.33292552453226421, -47.51618826727536771, 11.72657454140205679 ) ) ;
#4003 = CARTESIAN_POINT ( 'NONE',  ( -3.061616997868382155E-16, -39.99999999999997158, -99.20000000000000284 ) ) ;
#4004 = CIRCLE ( 'NONE', #6104, 7.499999999999999112 ) ;
#4005 = ORIENTED_EDGE ( 'NONE', *, *, #3131, .T. ) ;
#4006 = CARTESIAN_POINT ( 'NONE',  ( -31.39812190974910422, -40.95000000000000995, 8.827394325379140483 ) ) ;
#4007 = CARTESIAN_POINT ( 'NONE',  ( -39.84999999999998010, 22.00000000000000000, 80.00000000000002842 ) ) ;
#4008 =( BOUNDED_CURVE ( )  B_SPLINE_CURVE ( 2, ( #4684, #7370, #4025, #1908, #6702, #4773, #2706, #3369, #4595 ),
 .UNSPECIFIED., .F., .T. ) 
 B_SPLINE_CURVE_WITH_KNOTS ( ( 3, 2, 2, 2, 3 ),
 ( 0.7857142857142856984, 0.8035714285714286031, 0.8214285714285713969, 0.8392857142857144126, 0.8571428571428572063 ),
 .UNSPECIFIED. ) 
 CURVE ( )  GEOMETRIC_REPRESENTATION_ITEM ( )  RATIONAL_B_SPLINE_CURVE ( ( 1.000000000000000000, 0.9238795325112867385, 1.000000000000000000, 0.9238795325112867385, 1.000000000000000000, 0.9238795325112867385, 1.000000000000000000, 0.9238795325112862944, 1.000000000000000444 ) ) 
 REPRESENTATION_ITEM ( '' )  );
#4009 = ORIENTED_EDGE ( 'NONE', *, *, #5197, .F. ) ;
#4010 = CARTESIAN_POINT ( 'NONE',  ( 8.389419568037416259E-16, -49.56698729999997255, -99.24999999890751212 ) ) ;
#4011 = CARTESIAN_POINT ( 'NONE',  ( -4.999999999999998224, -42.92893218813448897, -97.34999999781506119 ) ) ;
#4012 = CARTESIAN_POINT ( 'NONE',  ( -38.46456197978948666, -47.40000000000001279, 4.312909747525784709 ) ) ;
#4013 = CARTESIAN_POINT ( 'NONE',  ( -1.891708078845683039, -40.43301269999998482, -97.79999999890752349 ) ) ;
#4014 = CARTESIAN_POINT ( 'NONE',  ( 42.00000000000000711, 21.99999999999992184, 60.00000000000002842 ) ) ;
#4015 = CARTESIAN_POINT ( 'NONE',  ( -21.61293655684001536, -30.20140427513057446, 1.382017864820032971 ) ) ;
#4016 = ADVANCED_FACE ( 'NONE', ( #4995 ), #4422, .F. ) ;
#4017 = CARTESIAN_POINT ( 'NONE',  ( 2.071067811865474173, -39.99999999999997158, -97.64300000002185698 ) ) ;
#4018 = VECTOR ( 'NONE', #7571, 1000.000000000000000 ) ;
#4019 = CARTESIAN_POINT ( 'NONE',  ( -36.01040764008574513, -33.00000000000000711, -6.010407640085605685 ) ) ;
#4020 = DIRECTION ( 'NONE',  ( 0.000000000000000000, 0.000000000000000000, 1.000000000000000000 ) ) ;
#4021 = DIRECTION ( 'NONE',  ( -0.5000000000000061062, 1.060575238724902601E-16, -0.8660254037844351549 ) ) ;
#4022 = ADVANCED_FACE ( 'NONE', ( #1738 ), #7315, .F. ) ;
#4023 = DIRECTION ( 'NONE',  ( -1.000000000000000000, 0.000000000000000000, 0.000000000000000000 ) ) ;
#4024 = ORIENTED_EDGE ( 'NONE', *, *, #6419, .F. ) ;
#4025 = CARTESIAN_POINT ( 'NONE',  ( 3.535533905932737309, -48.53553390593270933, -99.50000000000000000 ) ) ;
#4026 = CARTESIAN_POINT ( 'NONE',  ( -28.51387258211773812, -46.80000000000001137, 9.383039235653802379 ) ) ;
#4027 = CARTESIAN_POINT ( 'NONE',  ( -38.38706344316003793, -49.70140427513058512, -1.382017864820032083 ) ) ;
#4028 = DIRECTION ( 'NONE',  ( 1.000000000000000000, 0.000000000000000000, 0.000000000000000000 ) ) ;
#4029 = EDGE_CURVE ( 'NONE', #1100, #912, #4225, .T. ) ;
#4030 = CARTESIAN_POINT ( 'NONE',  ( 42.00000000000000711, 60.00000000000002842, 21.99999999999992184 ) ) ;
#4031 = CARTESIAN_POINT ( 'NONE',  ( -20.14280263777121149, -44.04859572486944330, -1.617624508639600833 ) ) ;
#4032 = CARTESIAN_POINT ( 'NONE',  ( 0.000000000000000000, 0.000000000000000000, 0.000000000000000000 ) ) ;
#4033 = CARTESIAN_POINT ( 'NONE',  ( -34.35889894354067309, 9.000000000000001776, 124.0000000000000000 ) ) ;
#4034 = CARTESIAN_POINT ( 'NONE',  ( -1.891708078845683483, -49.56698729999997255, -99.29999999890752349 ) ) ;
#4035 = VERTEX_POINT ( 'NONE', #1688 ) ;
#4036 = CARTESIAN_POINT ( 'NONE',  ( -23.68028341417693738, -45.74999999999999289, -6.319716585823198507 ) ) ;
#4037 = EDGE_CURVE ( 'NONE', #799, #2422, #2883, .T. ) ;
#4038 = CARTESIAN_POINT ( 'NONE',  ( -20.14280263777121149, -38.04859572486944330, -1.617624508639600833 ) ) ;
#4039 = CARTESIAN_POINT ( 'NONE',  ( -25.51477047955235378, -36.65140427513058086, 8.925456012876139766 ) ) ;
#4040 = ORIENTED_EDGE ( 'NONE', *, *, #5163, .T. ) ;
#4041 = VERTEX_POINT ( 'NONE', #2442 ) ;
#4042 = CARTESIAN_POINT ( 'NONE',  ( -28.56619749409589204, -45.80140427513057944, 9.391326687552490782 ) ) ;
#4043 = EDGE_CURVE ( 'NONE', #3192, #1887, #1108, .T. ) ;
#4044 = CARTESIAN_POINT ( 'NONE',  ( -41.99999999999996447, 60.00000000000002842, -20.35000000000000142 ) ) ;
#4045 = CARTESIAN_POINT ( 'NONE',  ( -2.071067811865475061, -39.99999999999997158, -99.84999999781504698 ) ) ;
#4046 = CARTESIAN_POINT ( 'NONE',  ( 5.000000000000000000, -47.07106781186545419, -96.25000000000000000 ) ) ;
#4047 = CARTESIAN_POINT ( 'NONE',  ( 5.000000000000000000, -47.07106781186545419, -98.65000000000000568 ) ) ;
#4048 = AXIS2_PLACEMENT_3D ( 'NONE', #7300, #1257, #3955 ) ;
#4049 = EDGE_LOOP ( 'NONE', ( #7756, #1721, #8051, #4848 ) ) ;
#4050 = VECTOR ( 'NONE', #708, 1000.000000000000000 ) ;
#4051 = CARTESIAN_POINT ( 'NONE',  ( -28.65689575858256077, -34.44859572486944188, -8.836108267985801845 ) ) ;
#4052 = CARTESIAN_POINT ( 'NONE',  ( -25.68709025247441602, -33.60000000000000142, -8.464561979789547053 ) ) ;
#4053 = EDGE_LOOP ( 'NONE', ( #4399, #5222, #3952, #6276 ) ) ;
#4054 = CARTESIAN_POINT ( 'NONE',  ( 4.566987300000000083, -46.89170807884564596, -98.29999999890752349 ) ) ;
#4055 = ADVANCED_FACE ( 'NONE', ( #8478 ), #5481, .F. ) ;
#4056 = CARTESIAN_POINT ( 'NONE',  ( 3.535533905932736420, -41.46446609406723383, -99.29999999999999716 ) ) ;
#4057 = CARTESIAN_POINT ( 'NONE',  ( -20.13408869516453947, -43.04999999999999005, -1.562606840307983136 ) ) ;
#4058 = AXIS2_PLACEMENT_3D ( 'NONE', #5867, #1861, #2399 ) ;
#4059 = CARTESIAN_POINT ( 'NONE',  ( 4.566987299999998307, -43.10829192115428299, -97.99999999890754054 ) ) ;
#4060 = EDGE_CURVE ( 'NONE', #3439, #3910, #6480, .T. ) ;
#4061 = CARTESIAN_POINT ( 'NONE',  ( -23.64089511245930098, -38.75140427513058228, -6.280328284105564762 ) ) ;
#4062 = SHAPE_REPRESENTATION ( 'sliding jaw', ( #2554 ), #1987 ) ;
#4063 = CARTESIAN_POINT ( 'NONE',  ( -2.071067811865475061, -39.99999999999997158, -95.94300000002186835 ) ) ;
#4064 = UNCERTAINTY_MEASURE_WITH_UNIT (LENGTH_MEASURE( 1.000000000000000082E-05 ), #7121, 'distance_accuracy_value', 'NONE');
#4065 = CARTESIAN_POINT ( 'NONE',  ( -23.98959235991431171, -43.50000000000001421, 6.010407640085604797 ) ) ;
#4066 = DIRECTION ( 'NONE',  ( 0.000000000000000000, 1.000000000000000000, 0.000000000000000000 ) ) ;
#4067 = CARTESIAN_POINT ( 'NONE',  ( 4.200000000000001954, 0.000000000000000000, 0.000000000000000000 ) ) ;
#4068 = ORIENTED_EDGE ( 'NONE', *, *, #6250, .T. ) ;
#4069 = DIRECTION ( 'NONE',  ( -1.000000000000000000, -0.000000000000000000, -0.000000000000000000 ) ) ;
#4070 = CARTESIAN_POINT ( 'NONE',  ( -22.93678734525658314, -48.75000000000001421, -7.063212654743582952 ) ) ;
#4071 = CARTESIAN_POINT ( 'NONE',  ( -24.02705286092866643, -45.50140427513058228, 6.047868141099968398 ) ) ;
#4072 = CARTESIAN_POINT ( 'NONE',  ( 4.999999999999998224, -44.99999999999997158, -96.20000000000000284 ) ) ;
#4073 = DIRECTION ( 'NONE',  ( 0.000000000000000000, 0.000000000000000000, -1.000000000000000000 ) ) ;
#4074 = CARTESIAN_POINT ( 'NONE',  ( -34.26570676250101855, -51.09859572486944046, 8.488613101951703044 ) ) ;
#4075 = DIRECTION ( 'NONE',  ( 0.000000000000000000, -0.5000000000000011102, -0.8660254037844379305 ) ) ;
#4076 = CARTESIAN_POINT ( 'NONE',  ( -34.53486167607238855, -33.15000000000000568, -8.900167166472096270 ) ) ;
#4077 =( LENGTH_UNIT ( ) NAMED_UNIT ( * ) SI_UNIT ( .MILLI., .METRE. ) );
#4078 = ORIENTED_EDGE ( 'NONE', *, *, #2678, .T. ) ;
#4079 = DIRECTION ( 'NONE',  ( -0.7071067811865587860, 0.000000000000000000, -0.7071067811865362485 ) ) ;
#4080 = CARTESIAN_POINT ( 'NONE',  ( -26.14108075221394856, -48.60000000000000142, -7.573555455601170827 ) ) ;
#4081 = CARTESIAN_POINT ( 'NONE',  ( -39.85719736222883824, -39.54859572486944330, 1.617624508639602388 ) ) ;
#4082 = CARTESIAN_POINT ( 'NONE',  ( -37.10260095646111012, -43.25140427513058228, 7.023824353025939438 ) ) ;
#4083 = VERTEX_POINT ( 'NONE', #5827 ) ;
#4084 = VERTEX_POINT ( 'NONE', #7728 ) ;
#4085 = CARTESIAN_POINT ( 'NONE',  ( -37.10260095646111012, -43.25140427513058228, 7.023824353025939438 ) ) ;
#4086 = SURFACE_STYLE_FILL_AREA ( #4706 ) ;
#4087 = CARTESIAN_POINT ( 'NONE',  ( -4.999999999999998224, -44.99999999999997158, -99.00000000000000000 ) ) ;
#4088 = AXIS2_PLACEMENT_3D ( 'NONE', #4287, #8136, #2095 ) ;
#4089 = CARTESIAN_POINT ( 'NONE',  ( 3.229347689422839895, -41.77065231057713390, -95.74999999890751212 ) ) ;
#4090 = CARTESIAN_POINT ( 'NONE',  ( 4.000000000000000000, 0.000000000000000000, 0.000000000000000000 ) ) ;
#4091 = FACE_BOUND ( 'NONE', #6510, .T. ) ;
#4092 = ORIENTED_EDGE ( 'NONE', *, *, #1008, .F. ) ;
#4093 = ADVANCED_FACE ( 'NONE', ( #4378 ), #8517, .F. ) ;
#4094 = CARTESIAN_POINT ( 'NONE',  ( -36.04786814110010340, -30.99859572486944259, -5.972947139071243861 ) ) ;
#4095 = CARTESIAN_POINT ( 'NONE',  ( -34.53486167607238144, -36.15000000000001279, -8.900167166472096270 ) ) ;
#4096 = EDGE_LOOP ( 'NONE', ( #1529, #3156, #424 ) ) ;
#4097 = ORIENTED_EDGE ( 'NONE', *, *, #3505, .T. ) ;
#4098 = CARTESIAN_POINT ( 'NONE',  ( 4.566987299999998307, -44.99999999999997158, -96.64999999890753202 ) ) ;
#4099 = CARTESIAN_POINT ( 'NONE',  ( 0.9662756667218486140, -39.99999999999997158, -100.0233279581959209 ) ) ;
#4100 = CARTESIAN_POINT ( 'NONE',  ( -39.38303923565386100, -47.70000000000000284, -1.486127417882099788 ) ) ;
#4101 = CARTESIAN_POINT ( 'NONE',  ( 3.229347689422839895, -41.77065231057713390, -99.54999999890752349 ) ) ;
#4102 = DIRECTION ( 'NONE',  ( -0.000000000000000000, 0.000000000000000000, 1.000000000000000000 ) ) ;
#4103 = CARTESIAN_POINT ( 'NONE',  ( -35.97294713907137975, -44.00140427513057517, -6.047868141099968398 ) ) ;
#4104 = MECHANICAL_DESIGN_GEOMETRIC_PRESENTATION_REPRESENTATION (  '', ( #8334 ), #7197 ) ;
#4105 = CARTESIAN_POINT ( 'NONE',  ( -2.071067811865475061, -39.99999999999997158, -95.14300000002184277 ) ) ;
#4106 = EDGE_CURVE ( 'NONE', #2506, #5578, #6312, .T. ) ;
#4107 = CARTESIAN_POINT ( 'NONE',  ( -28.67030704715798350, -40.80000000000000426, 8.395350895058669494 ) ) ;
#4108 = CARTESIAN_POINT ( 'NONE',  ( 26.02696727213731265, -48.05319586029025913, 11.85336373935252041 ) ) ;
#4109 = CARTESIAN_POINT ( 'NONE',  ( -36.71751442127229836, -51.00000000000000711, -6.717514421272142044 ) ) ;
#4110 = CONTEXT_DEPENDENT_SHAPE_REPRESENTATION ( #4535, #3746 ) ;
#4111 = ORIENTED_EDGE ( 'NONE', *, *, #2963, .F. ) ;
#4112 = FACE_BOUND ( 'NONE', #7350, .T. ) ;
#4113 = CARTESIAN_POINT ( 'NONE',  ( -28.51387258211773812, -49.80000000000001137, 9.383039235653802379 ) ) ;
#4114 = CARTESIAN_POINT ( 'NONE',  ( -24.02705286092866643, -48.50140427513058938, 6.047868141099968398 ) ) ;
#4115 = AXIS2_PLACEMENT_3D ( 'NONE', #5978, #8054, #7391 ) ;
#4116 = DIRECTION ( 'NONE',  ( 1.000000000000000000, 0.000000000000000000, 0.000000000000000000 ) ) ;
#4117 = CYLINDRICAL_SURFACE ( 'NONE', #6982, 4.999999999999969802 ) ;
#4118 = CARTESIAN_POINT ( 'NONE',  ( -39.39132668755255651, -42.69859572486944188, -1.433802505903950308 ) ) ;
#4119 = LINE ( 'NONE', #4161, #8176 ) ;
#4120 = CARTESIAN_POINT ( 'NONE',  ( -22.93678734525658314, -33.75000000000000711, -7.063212654743582064 ) ) ;
#4121 = AXIS2_PLACEMENT_3D ( 'NONE', #8056, #5398, #2020 ) ;
#4122 = ORIENTED_EDGE ( 'NONE', *, *, #5202, .T. ) ;
#4123 = DIRECTION ( 'NONE',  ( -1.000000000000000000, 0.000000000000000000, 0.000000000000000000 ) ) ;
#4124 = VERTEX_POINT ( 'NONE', #317 ) ;
#4125 = CARTESIAN_POINT ( 'NONE',  ( -36.01040764008574513, -51.00000000000000711, -6.010407640085605685 ) ) ;
#4126 = CARTESIAN_POINT ( 'NONE',  ( -21.55948914237271907, -37.89859572486944472, -4.360112732550413206 ) ) ;
#4127 = CARTESIAN_POINT ( 'NONE',  ( -39.87462524744216807, -40.55140427513058654, 1.507589171976367215 ) ) ;
#4128 = EDGE_CURVE ( 'NONE', #3779, #2752, #6046, .T. ) ;
#4129 = ORIENTED_EDGE ( 'NONE', *, *, #8100, .F. ) ;
#4130 = ORIENTED_EDGE ( 'NONE', *, *, #8544, .T. ) ;
#4131 = CARTESIAN_POINT ( 'NONE',  ( 8.389419568037416259E-16, -49.56698729999997255, -96.64999999890753202 ) ) ;
#4132 = CARTESIAN_POINT ( 'NONE',  ( -45.00000000000003553, -44.99999999999997158, -2.099999999999997868 ) ) ;
#4133 = CARTESIAN_POINT ( 'NONE',  ( -2.071067811865475505, -49.99999999999996447, -99.54999999781506403 ) ) ;
#4134 = CARTESIAN_POINT ( 'NONE',  ( 34.99999999999998579, -44.99999999999995737, -30.00100000000000122 ) ) ;
#4135 = FACE_BOUND ( 'NONE', #1401, .T. ) ;
#4136 = ORIENTED_EDGE ( 'NONE', *, *, #1709, .F. ) ;
#4137 = EDGE_CURVE ( 'NONE', #4270, #8652, #5515, .T. ) ;
#4138 = CARTESIAN_POINT ( 'NONE',  ( -28.65689575858256077, -31.44859572486944188, -8.836108267985801845 ) ) ;
#4139 = EDGE_CURVE ( 'NONE', #912, #1100, #5772, .T. ) ;
#4140 = CARTESIAN_POINT ( 'NONE',  ( -34.53486167607238144, -30.15000000000000213, -8.900167166472096270 ) ) ;
#4141 = ORIENTED_EDGE ( 'NONE', *, *, #2211, .F. ) ;
#4142 = CARTESIAN_POINT ( 'NONE',  ( 2.071067811865477282, -49.99999999999997158, -98.64999999781504414 ) ) ;
#4143 = CARTESIAN_POINT ( 'NONE',  ( -3.229347689422840784, -41.77065231057713390, -97.14999999890753202 ) ) ;
#4144 = AXIS2_PLACEMENT_3D ( 'NONE', #4695, #7380, #7507 ) ;
#4145 = CARTESIAN_POINT ( 'NONE',  ( 4.999999999999998224, -44.99999999999997158, -99.29999999781504982 ) ) ;
#4146 = DIRECTION ( 'NONE',  ( -1.000000000000000000, -0.000000000000000000, -0.000000000000000000 ) ) ;
#4147 = CARTESIAN_POINT ( 'NONE',  ( -2.796473189345805913E-16, -40.43301269999997061, -97.84999999890753486 ) ) ;
#4148 = FILL_AREA_STYLE ('',( #5324 ) ) ;
#4149 = CARTESIAN_POINT ( 'NONE',  ( -26.09387776718931917, -44.60140427513058370, -7.549504333439021941 ) ) ;
#4150 = EDGE_CURVE ( 'NONE', #5443, #1195, #408, .T. ) ;
#4151 = CARTESIAN_POINT ( 'NONE',  ( 2.071067811865477282, -49.99999999999996447, -98.74300000002187971 ) ) ;
#4152 = CARTESIAN_POINT ( 'NONE',  ( -36.01040764008574513, -45.00000000000000711, -6.010407640085605685 ) ) ;
#4153 = CYLINDRICAL_SURFACE ( 'NONE', #1587, 1.000000000000000888 ) ;
#4154 = CONTEXT_DEPENDENT_SHAPE_REPRESENTATION ( #193, #969 ) ;
#4155 = ORIENTED_EDGE ( 'NONE', *, *, #3542, .T. ) ;
#4156 = CARTESIAN_POINT ( 'NONE',  ( -49.99999999999997158, -59.99999999999997158, 30.00000000000000000 ) ) ;
#4157 = CARTESIAN_POINT ( 'NONE',  ( -20.61696076434619584, -46.20000000000000284, 1.486127417882100676 ) ) ;
#4158 = CARTESIAN_POINT ( 'NONE',  ( -26.14108075221394856, -33.60000000000000142, -7.573555455601170827 ) ) ;
#4159 = CARTESIAN_POINT ( 'NONE',  ( -28.68969400619928578, -40.16344083911688045, 12.43538147425380203 ) ) ;
#4160 = CARTESIAN_POINT ( 'NONE',  ( -20.14280263777121149, -50.04859572486944330, -1.617624508639600833 ) ) ;
#4161 = CARTESIAN_POINT ( 'NONE',  ( -50.00000000000002842, 30.00000000000000000, 80.00000000000002842 ) ) ;
#4162 = CARTESIAN_POINT ( 'NONE',  ( -34.31290974752564438, -35.10000000000000853, 8.464561979789547053 ) ) ;
#4163 =( NAMED_UNIT ( * ) PLANE_ANGLE_UNIT ( ) SI_UNIT ( $, .RADIAN. ) );
#4164 = EDGE_LOOP ( 'NONE', ( #1253, #7509, #7297, #5167 ) ) ;
#4165 = CARTESIAN_POINT ( 'NONE',  ( -3.535533905932735532, -48.53553390593270933, -98.90000000000000568 ) ) ;
#4166 = ORIENTED_EDGE ( 'NONE', *, *, #7092, .F. ) ;
#4167 = CARTESIAN_POINT ( 'NONE',  ( -21.60464910494133406, -46.20000000000000284, 1.329692952841886155 ) ) ;
#4168 = CARTESIAN_POINT ( 'NONE',  ( -28.49241082802385350, -37.44859572486943478, -9.874625247442173404 ) ) ;
#4169 = CARTESIAN_POINT ( 'NONE',  ( -34.36011273255026310, -40.10140427513057659, 8.440510857627391061 ) ) ;
#4170 = ADVANCED_FACE ( 'NONE', ( #7141 ), #3499, .T. ) ;
#4171 = EDGE_LOOP ( 'NONE', ( #4491, #5726 ) ) ;
#4172 = CARTESIAN_POINT ( 'NONE',  ( 3.229347689422841228, -48.22934768942280925, -95.74999999890752633 ) ) ;
#4173 = CARTESIAN_POINT ( 'NONE',  ( 50.00000000000002842, 60.00000000000002842, -30.00000000000000000 ) ) ;
#4174 = CARTESIAN_POINT ( 'NONE',  ( 4.566987300000000083, -46.89170807884565306, -96.69999999890752918 ) ) ;
#4175 = FACE_OUTER_BOUND ( 'NONE', #4801, .T. ) ;
#4176 = FACE_OUTER_BOUND ( 'NONE', #4607, .T. ) ;
#4177 = ORIENTED_EDGE ( 'NONE', *, *, #4888, .F. ) ;
#4178 = AXIS2_PLACEMENT_3D ( 'NONE', #4496, #6189, #5524 ) ;
#4179 = CARTESIAN_POINT ( 'NONE',  ( -23.98959235991431171, -49.50000000000000711, 6.010407640085604797 ) ) ;
#4180 = CARTESIAN_POINT ( 'NONE',  ( -39.86591130483550671, -35.55000000000001137, 1.562606840307984468 ) ) ;
#4181 = AXIS2_PLACEMENT_3D ( 'NONE', #6706, #7997, #6663 ) ;
#4182 = EDGE_LOOP ( 'NONE', ( #7335, #2027, #6805, #3831, #7640 ) ) ;
#4183 = CARTESIAN_POINT ( 'NONE',  ( -31.56260684030781505, -49.95000000000000995, 9.865911304835510265 ) ) ;
#4184 = CARTESIAN_POINT ( 'NONE',  ( -4.566987299999998307, -44.99999999999997158, -99.44999999890752918 ) ) ;
#4185 = ADVANCED_FACE ( 'NONE', ( #6453 ), #699, .F. ) ;
#4186 = CARTESIAN_POINT ( 'NONE',  ( 4.999999999999998224, -44.99999999999997158, -98.49999999781503845 ) ) ;
#4187 = CARTESIAN_POINT ( 'NONE',  ( 2.000000000000000000, 0.8865213383406717051, 1.535499999999999199 ) ) ;
#4188 = VECTOR ( 'NONE', #1243, 1000.000000000000000 ) ;
#4189 = CARTESIAN_POINT ( 'NONE',  ( 3.229347689422839895, -41.77065231057713390, -99.54999999890752349 ) ) ;
#4190 = CARTESIAN_POINT ( 'NONE',  ( -31.27736804086391942, -41.30140427513058654, -8.403638346957361449 ) ) ;
#4191 = CARTESIAN_POINT ( 'NONE',  ( -3.061616997868382155E-16, -39.99999999999997158, -96.00000000000000000 ) ) ;
#4192 = CARTESIAN_POINT ( 'NONE',  ( 1.891708078845682595, -40.43301269999998482, -96.29999999890752349 ) ) ;
#4193 = CARTESIAN_POINT ( 'NONE',  ( -33.85891924778610473, -47.10000000000000142, 7.573555455601171715 ) ) ;
#4194 = EDGE_CURVE ( 'NONE', #4208, #764, #1838, .T. ) ;
#4195 = CYLINDRICAL_SURFACE ( 'NONE', #466, 10.00000000000000178 ) ;
#4196 = ORIENTED_EDGE ( 'NONE', *, *, #4705, .T. ) ;
#4197 = CARTESIAN_POINT ( 'NONE',  ( -3.535533905932735532, -48.53553390593270933, -100.3999999978150441 ) ) ;
#4198 = FILL_AREA_STYLE ('',( #7541 ) ) ;
#4199 = EDGE_CURVE ( 'NONE', #5184, #1072, #5631, .T. ) ;
#4200 = CARTESIAN_POINT ( 'NONE',  ( -23.98959235991431171, -40.50000000000000711, 6.010407640085604797 ) ) ;
#4201 = CARTESIAN_POINT ( 'NONE',  ( 26.94471819803519708, -41.02872310104123699, 12.12402686769023141 ) ) ;
#4202 = CARTESIAN_POINT ( 'NONE',  ( -26.64110105645932336, 9.000000000000001776, 124.0000000000000000 ) ) ;
#4203 = CARTESIAN_POINT ( 'NONE',  ( -34.26570676250101855, -48.09859572486944046, 8.488613101951703044 ) ) ;
#4204 = DIRECTION ( 'NONE',  ( 0.000000000000000000, 0.000000000000000000, -1.000000000000000000 ) ) ;
#4205 = CARTESIAN_POINT ( 'NONE',  ( 42.00000000000000711, 60.00000000000002842, -21.99999999999992184 ) ) ;
#4206 = EDGE_LOOP ( 'NONE', ( #6811, #2145, #3748, #812 ) ) ;
#4207 = CARTESIAN_POINT ( 'NONE',  ( -30.00000000000002487, 0.000000000000000000, -25.00000000000000000 ) ) ;
#4208 = VERTEX_POINT ( 'NONE', #1120 ) ;
#4209 = CARTESIAN_POINT ( 'NONE',  ( -28.65689575858256077, -43.44859572486944188, -8.836108267985801845 ) ) ;
#4210 = CARTESIAN_POINT ( 'NONE',  ( -39.85719736222883824, -48.54859572486944330, 1.617624508639602388 ) ) ;
#4211 = CARTESIAN_POINT ( 'NONE',  ( -39.87462524744216807, -49.55140427513056522, 1.507589171976367215 ) ) ;
#4212 = ORIENTED_EDGE ( 'NONE', *, *, #5047, .T. ) ;
#4213 = CARTESIAN_POINT ( 'NONE',  ( -4.566987299999998307, -44.99999999999997158, -96.84999999890753486 ) ) ;
#4214 = EDGE_CURVE ( 'NONE', #7483, #5890, #2129, .T. ) ;
#4215 = DIRECTION ( 'NONE',  ( 0.000000000000000000, 0.000000000000000000, 1.000000000000000000 ) ) ;
#4216 = CARTESIAN_POINT ( 'NONE',  ( -33.76204298352917732, -41.69067313909257422, 11.92283337402248300 ) ) ;
#4217 = CARTESIAN_POINT ( 'NONE',  ( -2.796473189345805913E-16, -40.43301269999997061, -98.84999999890752065 ) ) ;
#4218 = CARTESIAN_POINT ( 'NONE',  ( -25.03224621535701289, -45.65699184524256538, 11.47067790983491875 ) ) ;
#4219 = FACE_BOUND ( 'NONE', #6629, .T. ) ;
#4220 = ORIENTED_EDGE ( 'NONE', *, *, #4323, .T. ) ;
#4221 = CARTESIAN_POINT ( 'NONE',  ( -22.45049566656107842, -31.89859572486943762, -3.906122232810846917 ) ) ;
#4222 = CARTESIAN_POINT ( 'NONE',  ( -25.68709025247441602, -36.60000000000000853, -8.464561979789547053 ) ) ;
#4223 = ORIENTED_EDGE ( 'NONE', *, *, #834, .F. ) ;
#4224 = CARTESIAN_POINT ( 'NONE',  ( -39.38303923565386100, -47.70000000000000284, -1.486127417882099788 ) ) ;
#4225 = CIRCLE ( 'NONE', #3529, 2.099999999999997868 ) ;
#4226 = DIRECTION ( 'NONE',  ( -0.000000000000000000, 1.000000000000000000, -0.000000000000000000 ) ) ;
#4227 = CARTESIAN_POINT ( 'NONE',  ( 4.566987300000000083, -46.89170807884564596, -99.89999999890751781 ) ) ;
#4228 = CARTESIAN_POINT ( 'NONE',  ( -2.071067811865475505, -49.99999999999996447, -100.3499999978150754 ) ) ;
#4229 = CARTESIAN_POINT ( 'NONE',  ( 2.000000000000000000, 1.773042676681340968, -1.951563910473907981E-15 ) ) ;
#4230 = CARTESIAN_POINT ( 'NONE',  ( -1.891708078845683039, -40.43301269999998482, -98.59999999890754907 ) ) ;
#4231 = EDGE_LOOP ( 'NONE', ( #1140, #4837, #5307, #8402 ) ) ;
#4232 = CARTESIAN_POINT ( 'NONE',  ( -36.35910488754074521, -46.25140427513058228, 6.280328284105565650 ) ) ;
#4233 = VECTOR ( 'NONE', #2892, 1000.000000000000000 ) ;
#4234 = EDGE_CURVE ( 'NONE', #8538, #6235, #6748, .T. ) ;
#4235 = CARTESIAN_POINT ( 'NONE',  ( -4.999999999999997335, -47.07106781186546129, -95.75000000000000000 ) ) ;
#4236 = PRODUCT_DEFINITION_CONTEXT ( 'detailed design', #6332, 'design' ) ;
#4237 = CARTESIAN_POINT ( 'NONE',  ( -4.566987299999998307, -43.10829192115428299, -96.89999999890751781 ) ) ;
#4238 = CARTESIAN_POINT ( 'NONE',  ( -21.60464910494133406, -49.20000000000000995, 1.329692952841886155 ) ) ;
#4239 = CARTESIAN_POINT ( 'NONE',  ( 39.99999999999996447, 1.102182119232617753E-14, 80.00000000000002842 ) ) ;
#4240 = SHAPE_DEFINITION_REPRESENTATION ( #990, #7097 ) ;
#4241 = DIRECTION ( 'NONE',  ( -1.000000000000000000, 0.000000000000000000, -0.000000000000000000 ) ) ;
#4242 = CARTESIAN_POINT ( 'NONE',  ( -21.17260567462091458, -34.04999999999998295, -1.398121909749242331 ) ) ;
#4243 = CARTESIAN_POINT ( 'NONE',  ( -27.77183716021333382, -40.51193879865776637, 12.30361675895773210 ) ) ;
#4244 = AXIS2_PLACEMENT_3D ( 'NONE', #2704, #1993, #3890 ) ;
#4245 = FACE_OUTER_BOUND ( 'NONE', #3107, .T. ) ;
#4246 = CARTESIAN_POINT ( 'NONE',  ( -22.93678734525658314, -33.75000000000001421, -7.063212654743582952 ) ) ;
#4247 = CARTESIAN_POINT ( 'NONE',  ( 2.071067811865477282, -49.99999999999997158, -97.95000000000000284 ) ) ;
#4248 = CARTESIAN_POINT ( 'NONE',  ( 3.535533905932737309, -48.53553390593270933, -99.39999999781504414 ) ) ;
#4249 =( REPRESENTATION_RELATIONSHIP ('NONE','NONE', #2265, #4062 ) REPRESENTATION_RELATIONSHIP_WITH_TRANSFORMATION ( #225 )SHAPE_REPRESENTATION_RELATIONSHIP( ) );
#4250 = SURFACE_STYLE_USAGE ( .BOTH. , #8183 ) ;
#4251 = ORIENTED_EDGE ( 'NONE', *, *, #3223, .T. ) ;
#4252 = CARTESIAN_POINT ( 'NONE',  ( -29.99999999999998579, 0.000000000000000000, -26.00000000000000355 ) ) ;
#4253 = ORIENTED_EDGE ( 'NONE', *, *, #2930, .T. ) ;
#4254 = CARTESIAN_POINT ( 'NONE',  ( -22.01140368885771892, -35.34859572486944046, 4.007875659808335378 ) ) ;
#4255 = CARTESIAN_POINT ( 'NONE',  ( -25.73429323749904185, -49.59859572486944046, -8.488613101951701267 ) ) ;
#4256 = CARTESIAN_POINT ( 'NONE',  ( -28.72263195913613387, -33.80140427513056522, 8.403638346957361449 ) ) ;
#4257 = ADVANCED_FACE ( 'NONE', ( #5839 ), #1038, .T. ) ;
#4258 = CARTESIAN_POINT ( 'NONE',  ( 3.229347689422839895, -41.77065231057713390, -96.34999999890753486 ) ) ;
#4259 = CARTESIAN_POINT ( 'NONE',  ( 42.00000000000000711, 21.99999999999992184, 80.00000000000002842 ) ) ;
#4260 = CIRCLE ( 'NONE', #1585, 1.535500000000000087 ) ;
#4261 = CARTESIAN_POINT ( 'NONE',  ( -32.65010723597040254, -40.75696118185769734, 12.21663313815758478 ) ) ;
#4262 = CARTESIAN_POINT ( 'NONE',  ( 4.566987299999998307, -44.99999999999997158, -96.64999999890753202 ) ) ;
#4263 = PLANE ( 'NONE',  #7804 ) ;
#4264 = DIRECTION ( 'NONE',  ( -0.000000000000000000, 1.000000000000000000, -0.000000000000000000 ) ) ;
#4265 = ORIENTED_EDGE ( 'NONE', *, *, #2496, .F. ) ;
#4266 = CARTESIAN_POINT ( 'NONE',  ( -33.81171626276147890, -42.09859572486944046, 7.597606577763319713 ) ) ;
#4267 = CARTESIAN_POINT ( 'NONE',  ( -36.71751442127229836, -42.00000000000000711, -6.717514421272142044 ) ) ;
#4268 = CIRCLE ( 'NONE', #1608, 10.00000000000000178 ) ;
#4269 = CONICAL_SURFACE ( 'NONE', #5526, 2.099999999999997868, 1.029744258676652313 ) ;
#4270 = VERTEX_POINT ( 'NONE', #369 ) ;
#4271 = CARTESIAN_POINT ( 'NONE',  ( -31.56260684030781505, -43.95000000000000284, 9.865911304835510265 ) ) ;
#4272 = LINE ( 'NONE', #7485, #1089 ) ;
#4273 = CARTESIAN_POINT ( 'NONE',  ( 3.535533905932736420, -41.46446609406723383, -99.99999999781503845 ) ) ;
#4274 = CARTESIAN_POINT ( 'NONE',  ( 0.000000000000000000, 4.163799117101000559E-16, -3.299999999999999822 ) ) ;
#4275 = CARTESIAN_POINT ( 'NONE',  ( 8.389419568037416259E-16, -49.56698729999997255, -99.84999999890753486 ) ) ;
#4276 = EDGE_LOOP ( 'NONE', ( #1927, #4092, #2391, #2334 ) ) ;
#4277 = CIRCLE ( 'NONE', #454, 4.999999999999973355 ) ;
#4278 = CARTESIAN_POINT ( 'NONE',  ( -22.03669253526174998, -31.34999999999999787, 4.057507815433014642 ) ) ;
#4279 = AXIS2_PLACEMENT_3D ( 'NONE', #4351, #952, #6325 ) ;
#4280 = CARTESIAN_POINT ( 'NONE',  ( -4.999999999999997335, -47.07106781186546129, -98.94300000002183992 ) ) ;
#4281 = DIRECTION ( 'NONE',  ( 0.000000000000000000, 0.000000000000000000, -1.000000000000000000 ) ) ;
#4282 = CARTESIAN_POINT ( 'NONE',  ( -45.00000000000003553, -44.99999999999997158, 0.000000000000000000 ) ) ;
#4283 = DIRECTION ( 'NONE',  ( 1.000000000000000000, 0.000000000000000000, 0.000000000000000000 ) ) ;
#4284 = DIRECTION ( 'NONE',  ( 0.000000000000000000, 0.000000000000000000, -1.000000000000000000 ) ) ;
#4285 = CARTESIAN_POINT ( 'NONE',  ( -22.03669253526174998, -34.35000000000000853, 4.057507815433014642 ) ) ;
#4286 = CARTESIAN_POINT ( 'NONE',  ( 27.77933658956289520, -40.51720970344479866, 12.30204028087673152 ) ) ;
#4287 = CARTESIAN_POINT ( 'NONE',  ( 50.00000000000002842, -44.99999999999997158, 0.000000000000000000 ) ) ;
#4288 = CARTESIAN_POINT ( 'NONE',  ( -34.31290974752564438, -35.10000000000000853, 8.464561979789547053 ) ) ;
#4289 = ADVANCED_FACE ( 'NONE', ( #5753 ), #8452, .T. ) ;
#4290 = CARTESIAN_POINT ( 'NONE',  ( -4.999999999999997335, -47.07106781186546129, -98.15000000000000568 ) ) ;
#4291 = CARTESIAN_POINT ( 'NONE',  ( -22.93678734525658314, -36.75000000000000711, -7.063212654743582064 ) ) ;
#4292 = ORIENTED_EDGE ( 'NONE', *, *, #6522, .T. ) ;
#4293 = DIRECTION ( 'NONE',  ( -0.000000000000000000, -0.000000000000000000, 1.000000000000000000 ) ) ;
#4294 = ORIENTED_EDGE ( 'NONE', *, *, #4234, .F. ) ;
#4295 = CARTESIAN_POINT ( 'NONE',  ( -26.18828373723858149, -34.59859572486944046, -7.597606577763319713 ) ) ;
#4296 = CARTESIAN_POINT ( 'NONE',  ( -25.41550616830297571, -47.64859572486945183, 8.874878320068054549 ) ) ;
#4297 = CARTESIAN_POINT ( 'NONE',  ( -37.10260095646111012, -49.25140427513058938, 7.023824353025939438 ) ) ;
#4298 = ADVANCED_FACE ( 'NONE', ( #7869 ), #7118, .T. ) ;
#4299 = CARTESIAN_POINT ( 'NONE',  ( -1.891708078845683039, -40.43301269999998482, -97.79999999890752349 ) ) ;
#4300 = CARTESIAN_POINT ( 'NONE',  ( -4.999999999999998224, -44.99999999999997158, -99.79999999999999716 ) ) ;
#4301 = CARTESIAN_POINT ( 'NONE',  ( -30.32897932148009801, -40.00000000000001421, 12.49999999999998046 ) ) ;
#4302 = CARTESIAN_POINT ( 'NONE',  ( 8.389419568037416259E-16, -49.56698729999997255, -99.24999999890751212 ) ) ;
#4303 = CARTESIAN_POINT ( 'NONE',  ( -27.76868453341328546, -49.48665499171480775, 12.30309571437652671 ) ) ;
#4304 = CONICAL_SURFACE ( 'NONE', #1631, 1.535500000000000087, 1.047197551196590748 ) ;
#4305 = CARTESIAN_POINT ( 'NONE',  ( -4.566987299999998307, -43.10829192115428299, -96.29999999890752349 ) ) ;
#4306 = EDGE_CURVE ( 'NONE', #7279, #58, #2454, .T. ) ;
#4307 = DIRECTION ( 'NONE',  ( 1.000000000000000000, 0.000000000000000000, 0.000000000000000000 ) ) ;
#4308 = ORIENTED_EDGE ( 'NONE', *, *, #2286, .F. ) ;
#4309 = CARTESIAN_POINT ( 'NONE',  ( -31.38201786482021305, -37.29859572486943620, -8.387063443159975762 ) ) ;
#4310 = CARTESIAN_POINT ( 'NONE',  ( -28.51387258211773812, -46.80000000000001137, 9.383039235653802379 ) ) ;
#4311 = VERTEX_POINT ( 'NONE', #5135 ) ;
#4312 = AXIS2_PLACEMENT_3D ( 'NONE', #1348, #3217, #8108 ) ;
#4313 = CARTESIAN_POINT ( 'NONE',  ( -28.43739315969223824, -45.45000000000000995, -9.865911304835512041 ) ) ;
#4314 =( LENGTH_UNIT ( ) NAMED_UNIT ( * ) SI_UNIT ( .MILLI., .METRE. ) );
#4315 = CARTESIAN_POINT ( 'NONE',  ( -5.000000000000007994, -42.92893218813450318, -98.14999999781504414 ) ) ;
#4316 = CARTESIAN_POINT ( 'NONE',  ( 3.535533905932737309, -48.53553390593270933, -99.39999999781504414 ) ) ;
#4317 = CIRCLE ( 'NONE', #5723, 2.149999999999985256 ) ;
#4318 = DIRECTION ( 'NONE',  ( -0.000000000000000000, -0.000000000000000000, 1.000000000000000000 ) ) ;
#4319 = CARTESIAN_POINT ( 'NONE',  ( -1.891708078845683483, -49.56698729999997255, -98.29999999890752349 ) ) ;
#4320 = PRODUCT_DEFINITION ( 'UNKNOWN', '', #20, #425 ) ;
#4321 = ORIENTED_EDGE ( 'NONE', *, *, #504, .T. ) ;
#4322 = CARTESIAN_POINT ( 'NONE',  ( -31.32969295284206979, -33.30000000000000426, -8.395350895058669494 ) ) ;
#4323 = EDGE_CURVE ( 'NONE', #6099, #6319, #4674, .T. ) ;
#4324 = AXIS2_PLACEMENT_3D ( 'NONE', #2710, #4691, #7907 ) ;
#4325 = CARTESIAN_POINT ( 'NONE',  ( -3.061616997868382155E-16, -39.99999999999997158, -95.20000000000000284 ) ) ;
#4326 = DIRECTION ( 'NONE',  ( 0.000000000000000000, 0.000000000000000000, -1.000000000000000000 ) ) ;
#4327 = EDGE_CURVE ( 'NONE', #6070, #1128, #4693, .T. ) ;
#4328 = CARTESIAN_POINT ( 'NONE',  ( -2.071067811865475061, -39.99999999999997158, -97.44999999781505551 ) ) ;
#4329 = LINE ( 'NONE', #7625, #8600 ) ;
#4330 = AXIS2_PLACEMENT_3D ( 'NONE', #3914, #2063, #7435 ) ;
#4331 = CARTESIAN_POINT ( 'NONE',  ( -2.071067811865475061, -39.99999999999997158, -100.6499999978150441 ) ) ;
#4332 = VECTOR ( 'NONE', #7856, 1000.000000000000000 ) ;
#4333 = CARTESIAN_POINT ( 'NONE',  ( -37.96330746473829976, -41.84999999999999432, -4.057507815433013754 ) ) ;
#4334 = CARTESIAN_POINT ( 'NONE',  ( -30.00000000000002842, 0.000000000000000000, -45.00000000000000000 ) ) ;
#4335 = DIRECTION ( 'NONE',  ( 0.000000000000000000, 0.000000000000000000, 1.000000000000000000 ) ) ;
#4336 = CARTESIAN_POINT ( 'NONE',  ( -23.28248557872775137, -34.50000000000000000, 6.717514421272141156 ) ) ;
#4337 = CARTESIAN_POINT ( 'NONE',  ( 45.00000000000003553, -44.99999999999997158, 2.099999999999997868 ) ) ;
#4338 = CARTESIAN_POINT ( 'NONE',  ( -31.48612741788231517, -45.30000000000000426, -9.383039235653804155 ) ) ;
#4339 = VECTOR ( 'NONE', #3228, 1000.000000000000000 ) ;
#4340 = VERTEX_POINT ( 'NONE', #3243 ) ;
#4341 = FACE_OUTER_BOUND ( 'NONE', #8236, .T. ) ;
#4342 = EDGE_LOOP ( 'NONE', ( #4223, #4831, #1769, #4395 ) ) ;
#4343 = CARTESIAN_POINT ( 'NONE',  ( -36.04786814110010340, -36.99859572486943193, -5.972947139071243861 ) ) ;
#4344 = CARTESIAN_POINT ( 'NONE',  ( -31.53845232986046554, -46.29859572486944330, -9.374751783755117529 ) ) ;
#4345 = CARTESIAN_POINT ( 'NONE',  ( -39.37475178375516549, -46.70140427513057801, -1.538452329860249712 ) ) ;
#4346 =( BOUNDED_CURVE ( )  B_SPLINE_CURVE ( 2, ( #6929, #4825, #1553, #4247, #1468, #2273, #7634, #4290, #1424 ),
 .UNSPECIFIED., .F., .T. ) 
 B_SPLINE_CURVE_WITH_KNOTS ( ( 3, 2, 2, 2, 3 ),
 ( 0.5000000000000000000, 0.5178571428571429047, 0.5357142857142856984, 0.5535714285714286031, 0.5714285714285713969 ),
 .UNSPECIFIED. ) 
 CURVE ( )  GEOMETRIC_REPRESENTATION_ITEM ( )  RATIONAL_B_SPLINE_CURVE ( ( 1.000000000000000000, 0.9238795325112867385, 1.000000000000000000, 0.9238795325112867385, 1.000000000000000000, 0.9238795325112867385, 1.000000000000000000, 0.9238795325112867385, 1.000000000000000000 ) ) 
 REPRESENTATION_ITEM ( '' )  );
#4347 = CARTESIAN_POINT ( 'NONE',  ( 4.566987300000000083, -46.89170807884564596, -99.69999999890752918 ) ) ;
#4348 = FACE_OUTER_BOUND ( 'NONE', #8270, .T. ) ;
#4349 = PRODUCT_DEFINITION_SHAPE ( 'NONE', 'NONE',  #8730 ) ;
#4350 = CARTESIAN_POINT ( 'NONE',  ( -4.566987299999997418, -46.89170807884566727, -97.79999999890752349 ) ) ;
#4351 = CARTESIAN_POINT ( 'NONE',  ( -30.00000000000002842, 0.000000000000000000, -45.00000000000000000 ) ) ;
#4352 = CARTESIAN_POINT ( 'NONE',  ( -4.566987299999998307, -44.99999999999997158, -97.04999999890752349 ) ) ;
#4353 = CARTESIAN_POINT ( 'NONE',  ( -2.796473189345805913E-16, -40.43301269999997061, -100.4499999989075292 ) ) ;
#4354 = VERTEX_POINT ( 'NONE', #2048 ) ;
#4355 = CLOSED_SHELL ( 'NONE', ( #2469, #1232, #5692, #5149, #966, #4465, #606, #6106, #8706, #8561, #5704, #1353, #6759, #3416, #4298, #8603, #3716, #413, #929, #7051, #5600, #5855, #3262, #4504, #1274, #2736, #6072 ) ) ;
#4356 = CARTESIAN_POINT ( 'NONE',  ( -23.71967171589458445, -43.74859572486943904, -6.359104887540838469 ) ) ;
#4357 = CARTESIAN_POINT ( 'NONE',  ( -34.31290974752564438, -47.10000000000000142, 8.464561979789547053 ) ) ;
#4358 = ORIENTED_EDGE ( 'NONE', *, *, #1723, .F. ) ;
#4359 = CARTESIAN_POINT ( 'NONE',  ( -28.51387258211773812, -43.80000000000000426, 9.383039235653802379 ) ) ;
#4360 = CARTESIAN_POINT ( 'NONE',  ( -34.33694741576523768, -47.50955795526805048, 11.72510588894414596 ) ) ;
#4361 = CARTESIAN_POINT ( 'NONE',  ( 2.071067811865474173, -39.99999999999997158, -98.34999999781506119 ) ) ;
#4362 = DIRECTION ( 'NONE',  ( -0.000000000000000000, 1.000000000000000000, -0.000000000000000000 ) ) ;
#4363 = PLANE ( 'NONE',  #2867 ) ;
#4364 = CARTESIAN_POINT ( 'NONE',  ( -4.999999999999998224, -44.99999999999997158, -96.60000000000000853 ) ) ;
#4365 = EDGE_LOOP ( 'NONE', ( #7539, #4097, #5986, #7889, #5674 ) ) ;
#4366 = CARTESIAN_POINT ( 'NONE',  ( -37.57355545560112375, -32.40000000000000568, 3.858919247786223305 ) ) ;
#4367 = EDGE_LOOP ( 'NONE', ( #6754, #7523, #1519, #4358 ) ) ;
#4368 = APPLICATION_CONTEXT ( 'automotive_design' ) ;
#4369 = PLANE ( 'NONE',  #3885 ) ;
#4370 = CARTESIAN_POINT ( 'NONE',  ( 2.071067811865474173, -39.99999999999997158, -97.54999999781504982 ) ) ;
#4371 = VECTOR ( 'NONE', #1821, 1000.000000000000000 ) ;
#4372 = LINE ( 'NONE', #4990, #6114 ) ;
#4373 = CARTESIAN_POINT ( 'NONE',  ( -41.99999999999981526, 0.000000000000000000, -29.65000000000000213 ) ) ;
#4374 = CARTESIAN_POINT ( 'NONE',  ( -25.94249218456686279, -40.65000000000000568, 7.963307464738195840 ) ) ;
#4375 = PRODUCT_DEFINITION_SHAPE ( 'NONE', 'NONE',  #8718 ) ;
#4376 = CARTESIAN_POINT ( 'NONE',  ( 2.071067811865477282, -49.99999999999997158, -97.04999999781504982 ) ) ;
#4377 = CARTESIAN_POINT ( 'NONE',  ( -25.00000000000002487, -45.00000000000000000, 11.45643923738959025 ) ) ;
#4378 = FACE_OUTER_BOUND ( 'NONE', #5762, .T. ) ;
#4379 = CARTESIAN_POINT ( 'NONE',  ( -20.61696076434619584, -37.20000000000000284, 1.486127417882100676 ) ) ;
#4380 = CARTESIAN_POINT ( 'NONE',  ( 0.1999999999999987899, 0.000000000000000000, 3.500000000000000000 ) ) ;
#4381 = AXIS2_PLACEMENT_3D ( 'NONE', #7492, #4808, #1616 ) ;
#4382 = CARTESIAN_POINT ( 'NONE',  ( -34.53486167607238855, -42.15000000000000568, -8.900167166472096270 ) ) ;
#4383 = SURFACE_SIDE_STYLE ('',( #1693 ) ) ;
#4384 = ORIENTED_EDGE ( 'NONE', *, *, #1630, .T. ) ;
#4385 = EDGE_LOOP ( 'NONE', ( #6262, #5530, #4712, #6135 ) ) ;
#4386 = CARTESIAN_POINT ( 'NONE',  ( -21.59636165304264921, -47.19859572486943478, 1.277368040863740228 ) ) ;
#4387 = CARTESIAN_POINT ( 'NONE',  ( -28.43739315969223824, -30.44999999999999574, -9.865911304835512041 ) ) ;
#4388 = CARTESIAN_POINT ( 'NONE',  ( -37.59760657776328685, -34.40140427513058086, 3.811716262761598362 ) ) ;
#4389 = CARTESIAN_POINT ( 'NONE',  ( -3.229347689422839451, -48.22934768942280925, -99.14999999890753202 ) ) ;
#4390 = FACE_OUTER_BOUND ( 'NONE', #3457, .T. ) ;
#4391 = CARTESIAN_POINT ( 'NONE',  ( -21.09983283352784156, -34.35000000000000853, 4.534861676072186043 ) ) ;
#4392 = CARTESIAN_POINT ( 'NONE',  ( -30.00000000000000000, -49.99999999999997158, 0.000000000000000000 ) ) ;
#4393 = DIRECTION ( 'NONE',  ( 0.000000000000000000, -1.000000000000000000, 0.000000000000000000 ) ) ;
#4394 = CARTESIAN_POINT ( 'NONE',  ( -4.566987299999998307, -43.10829192115428299, -95.49999999890754054 ) ) ;
#4395 = ORIENTED_EDGE ( 'NONE', *, *, #6699, .F. ) ;
#4396 = SHAPE_REPRESENTATION ( 'guide block', ( #2554 ), #7190 ) ;
#4397 = CARTESIAN_POINT ( 'NONE',  ( -21.18131961722757595, -41.04859572486944330, -1.453139578080854699 ) ) ;
#4398 = CARTESIAN_POINT ( 'NONE',  ( -39.38303923565386100, -47.70000000000000284, -1.486127417882099788 ) ) ;
#4399 = ORIENTED_EDGE ( 'NONE', *, *, #99, .T. ) ;
#4400 = CIRCLE ( 'NONE', #7914, 2.000000000000001776 ) ;
#4401 = CARTESIAN_POINT ( 'NONE',  ( -28.38237549136062654, -32.45140427513058512, -9.857197362228843573 ) ) ;
#4402 = CARTESIAN_POINT ( 'NONE',  ( -2.071067811865475061, -39.99999999999997158, -96.64999999781505835 ) ) ;
#4403 = CARTESIAN_POINT ( 'NONE',  ( 44.14999999999999147, -21.99999999999992184, 60.00000000000002842 ) ) ;
#4404 = CARTESIAN_POINT ( 'NONE',  ( -3.535533905932735532, -48.53553390593270933, -95.70000000000000284 ) ) ;
#4405 = LINE ( 'NONE', #8466, #6646 ) ;
#4406 = CARTESIAN_POINT ( 'NONE',  ( -4.999999999999998224, -44.99999999999997158, -95.00000000000000000 ) ) ;
#4407 = EDGE_CURVE ( 'NONE', #6544, #2302, #6619, .T. ) ;
#4408 = VERTEX_POINT ( 'NONE', #714 ) ;
#4409 = CARTESIAN_POINT ( 'NONE',  ( -21.17260567462091458, -37.05000000000001137, -1.398121909749242331 ) ) ;
#4410 = AXIS2_PLACEMENT_3D ( 'NONE', #6857, #4924, #5622 ) ;
#4411 = CIRCLE ( 'NONE', #3570, 0.2000000000000000944 ) ;
#4412 = ORIENTED_EDGE ( 'NONE', *, *, #5387, .T. ) ;
#4413 = CARTESIAN_POINT ( 'NONE',  ( 2.071067811865474173, -39.99999999999997158, -98.44999999999998863 ) ) ;
#4414 = AXIS2_PLACEMENT_3D ( 'NONE', #3122, #3863, #6541 ) ;
#4415 = CARTESIAN_POINT ( 'NONE',  ( 9.184850993605145972E-16, -49.99999999999997158, -97.89999999781504414 ) ) ;
#4416 = FACE_OUTER_BOUND ( 'NONE', #1427, .T. ) ;
#4417 = EDGE_CURVE ( 'NONE', #4041, #2323, #3938, .T. ) ;
#4418 = DIRECTION ( 'NONE',  ( 0.000000000000000000, 0.000000000000000000, 1.000000000000000000 ) ) ;
#4419 = CARTESIAN_POINT ( 'NONE',  ( -23.98959235991431171, -43.50000000000001421, 6.010407640085604797 ) ) ;
#4420 = DIRECTION ( 'NONE',  ( 0.000000000000000000, 0.000000000000000000, 1.000000000000000000 ) ) ;
#4421 = CARTESIAN_POINT ( 'NONE',  ( -25.64110105645932336, -7.999999999999996447, -24.00000000000000000 ) ) ;
#4422 = CYLINDRICAL_SURFACE ( 'NONE', #2401, 1.649999999999998579 ) ;
#4423 = CARTESIAN_POINT ( 'NONE',  ( -38.90016716647221529, -38.85000000000001563, -4.534861676072185155 ) ) ;
#4424 = VECTOR ( 'NONE', #8001, 1000.000000000000000 ) ;
#4425 = DIRECTION ( 'NONE',  ( -0.000000000000000000, -0.000000000000000000, -1.000000000000000000 ) ) ;
#4426 = CARTESIAN_POINT ( 'NONE',  ( -25.68709025247441602, -42.60000000000000853, -8.464561979789547053 ) ) ;
#4427 = PRODUCT_RELATED_PRODUCT_CATEGORY ( 'part', '', ( #2345 ) ) ;
#4428 = EDGE_LOOP ( 'NONE', ( #1173, #210, #7022, #6852 ) ) ;
#4429 = CARTESIAN_POINT ( 'NONE',  ( -38.40363834695740053, -51.69859572486944188, -1.277368040863739118 ) ) ;
#4430 = CARTESIAN_POINT ( 'NONE',  ( -31.48612741788231517, -39.30000000000001137, -9.383039235653804155 ) ) ;
#4431 = CARTESIAN_POINT ( 'NONE',  ( -31.27736804086391942, -35.30140427513057944, -8.403638346957361449 ) ) ;
#4432 = CARTESIAN_POINT ( 'NONE',  ( 1.891708078845685481, -49.56698729999997255, -98.99999999890752633 ) ) ;
#4433 = DIRECTION ( 'NONE',  ( 0.000000000000000000, 0.000000000000000000, -1.000000000000000000 ) ) ;
#4434 = CARTESIAN_POINT ( 'NONE',  ( -31.48612741788231517, -33.30000000000000426, -9.383039235653804155 ) ) ;
#4435 = CARTESIAN_POINT ( 'NONE',  ( -4.566987299999998307, -44.99999999999997158, -99.44999999890752918 ) ) ;
#4436 = CARTESIAN_POINT ( 'NONE',  ( 45.00000000000003553, -44.99999999999997158, 0.000000000000000000 ) ) ;
#4437 = CARTESIAN_POINT ( 'NONE',  ( 4.566987299999998307, -43.10829192115428299, -97.39999999890751781 ) ) ;
#4438 = SURFACE_STYLE_FILL_AREA ( #5138 ) ;
#4439 = EDGE_LOOP ( 'NONE', ( #3959, #1388, #6582, #463 ) ) ;
#4440 = DIRECTION ( 'NONE',  ( -0.000000000000000000, 1.000000000000000000, -0.000000000000000000 ) ) ;
#4441 = CARTESIAN_POINT ( 'NONE',  ( -37.98859631114233792, -36.84859572486944046, -4.007875659808334490 ) ) ;
#4442 = CARTESIAN_POINT ( 'NONE',  ( -28.43739315969223824, -42.44999999999999574, -9.865911304835512041 ) ) ;
#4443 = ORIENTED_EDGE ( 'NONE', *, *, #778, .T. ) ;
#4444 = CARTESIAN_POINT ( 'NONE',  ( -34.36011273255026310, -31.10140427513058370, 8.440510857627391061 ) ) ;
#4445 = FACE_OUTER_BOUND ( 'NONE', #4937, .T. ) ;
#4446 = DIRECTION ( 'NONE',  ( 0.000000000000000000, -0.5000000000000011102, -0.8660254037844379305 ) ) ;
#4447 = LINE ( 'NONE', #1806, #7068 ) ;
#4448 = CARTESIAN_POINT ( 'NONE',  ( 2.000000000000000000, 0.000000000000000000, 0.000000000000000000 ) ) ;
#4449 = CARTESIAN_POINT ( 'NONE',  ( -3.535533905932735532, -48.53553390593270933, -96.50000000000000000 ) ) ;
#4450 = EDGE_LOOP ( 'NONE', ( #5563, #7962, #3091 ) ) ;
#4451 = CARTESIAN_POINT ( 'NONE',  ( -28.72263195913613387, -48.80140427513057233, 8.403638346957361449 ) ) ;
#4452 = EDGE_CURVE ( 'NONE', #4683, #7457, #1205, .T. ) ;
#4453 = VERTEX_POINT ( 'NONE', #5338 ) ;
#4454 = CARTESIAN_POINT ( 'NONE',  ( -4.999999999999997335, -47.07106781186546129, -98.15000000000000568 ) ) ;
#4455 = CARTESIAN_POINT ( 'NONE',  ( 5.000000000000000000, -47.07106781186545419, -97.74999999781503845 ) ) ;
#4456 = CARTESIAN_POINT ( 'NONE',  ( -4.135692067460690069, -42.17523997218626874, -100.0007971519677881 ) ) ;
#4457 = AXIS2_PLACEMENT_3D ( 'NONE', #5158, #2849, #2188 ) ;
#4458 = CARTESIAN_POINT ( 'NONE',  ( 0.000000000000000000, -44.99999999999997158, -95.00000000000000000 ) ) ;
#4459 = FACE_OUTER_BOUND ( 'NONE', #4551, .T. ) ;
#4460 = DIRECTION ( 'NONE',  ( -1.000000000000000000, -0.000000000000000000, -0.000000000000000000 ) ) ;
#4461 = CIRCLE ( 'NONE', #5869, 10.00000000000000178 ) ;
#4462 = FACE_OUTER_BOUND ( 'NONE', #7253, .T. ) ;
#4463 = CARTESIAN_POINT ( 'NONE',  ( -31.48612741788231517, -42.30000000000000426, -9.383039235653804155 ) ) ;
#4464 = AXIS2_PLACEMENT_3D ( 'NONE', #6745, #4069, #6791 ) ;
#4465 = ADVANCED_FACE ( 'NONE', ( #6008 ), #8698, .T. ) ;
#4466 = ORIENTED_EDGE ( 'NONE', *, *, #1671, .T. ) ;
#4467 = CARTESIAN_POINT ( 'NONE',  ( -20.60867331244750034, -32.19859572486942767, 1.433802505903951419 ) ) ;
#4468 = CARTESIAN_POINT ( 'NONE',  ( -38.90016716647221529, -38.85000000000001563, -4.534861676072185155 ) ) ;
#4469 = CARTESIAN_POINT ( 'NONE',  ( -31.45313957808072303, -42.95140427513058512, 8.818680382772479120 ) ) ;
#4470 = CARTESIAN_POINT ( 'NONE',  ( 1.891708078845682595, -40.43301269999998482, -98.69999999890752918 ) ) ;
#4471 = UNCERTAINTY_MEASURE_WITH_UNIT (LENGTH_MEASURE( 1.000000000000000082E-05 ), #7559, 'distance_accuracy_value', 'NONE');
#4472 = DIRECTION ( 'NONE',  ( 0.000000000000000000, 0.000000000000000000, 1.000000000000000000 ) ) ;
#4473 = CARTESIAN_POINT ( 'NONE',  ( -39.86591130483550671, -38.54999999999999716, 1.562606840307984468 ) ) ;
#4474 = DIRECTION ( 'NONE',  ( -1.000000000000000000, 0.000000000000000000, 0.000000000000000000 ) ) ;
#4475 = DIRECTION ( 'NONE',  ( 0.000000000000000000, 0.000000000000000000, -1.000000000000000000 ) ) ;
#4476 = CARTESIAN_POINT ( 'NONE',  ( -2.796473189345805913E-16, -40.43301269999997061, -95.64999999890753202 ) ) ;
#4477 = SHAPE_REPRESENTATION_RELATIONSHIP ( 'NONE' , 'NONE' ,  #6809, #2657 ) ;
#4478 = EDGE_LOOP ( 'NONE', ( #5218, #4702, #5155, #1371 ) ) ;
#4479 = LINE ( 'NONE', #8456, #5952 ) ;
#4480 = CARTESIAN_POINT ( 'NONE',  ( -21.18131961722757595, -47.04859572486944330, -1.453139578080854699 ) ) ;
#4481 = CARTESIAN_POINT ( 'NONE',  ( -34.48522952044771017, -29.15140427513058441, -8.925456012876139766 ) ) ;
#4482 = ORIENTED_EDGE ( 'NONE', *, *, #5318, .F. ) ;
#4483 = CARTESIAN_POINT ( 'NONE',  ( -38.48861310195163554, -34.40140427513058086, 4.265706762501153548 ) ) ;
#4484 = ADVANCED_FACE ( 'NONE', ( #2759 ), #6752, .T. ) ;
#4485 = CARTESIAN_POINT ( 'NONE',  ( -4.999999999999998224, -44.99999999999997158, -95.69999999781504130 ) ) ;
#4486 = CARTESIAN_POINT ( 'NONE',  ( -30.00000000000002487, 0.000000000000000000, -45.00000000000000000 ) ) ;
#4487 = CARTESIAN_POINT ( 'NONE',  ( -4.999999999999994671, -47.07106781186545419, -95.75000000000000000 ) ) ;
#4488 = DIRECTION ( 'NONE',  ( 0.000000000000000000, 0.000000000000000000, -1.000000000000000000 ) ) ;
#4489 = CARTESIAN_POINT ( 'NONE',  ( -3.061616997868382155E-16, -39.99999999999997158, -96.79999999999999716 ) ) ;
#4490 = CLOSED_SHELL ( 'NONE', ( #2026, #1818, #177, #6872, #3943, #3836, #5424, #3349, #7858, #1444, #1836, #5731, #3651, #2745, #5818, #6131, #904, #8 ) ) ;
#4491 = ORIENTED_EDGE ( 'NONE', *, *, #4736, .F. ) ;
#4492 = CARTESIAN_POINT ( 'NONE',  ( -26.14108075221394856, -42.60000000000000853, -7.573555455601170827 ) ) ;
#4493 = ORIENTED_EDGE ( 'NONE', *, *, #4779, .T. ) ;
#4494 = CARTESIAN_POINT ( 'NONE',  ( -4.999999999999998224, -44.99999999999997158, -98.19999999999998863 ) ) ;
#4495 = CARTESIAN_POINT ( 'NONE',  ( -41.99999999999996447, 60.00000000000002842, -22.00000000000000000 ) ) ;
#4496 = CARTESIAN_POINT ( 'NONE',  ( -49.99999999999997158, -59.99999999999997158, 30.00000000000000000 ) ) ;
#4497 = EDGE_CURVE ( 'NONE', #899, #6389, #135, .T. ) ;
#4498 = CARTESIAN_POINT ( 'NONE',  ( 0.000000000000000000, -44.99999999999997158, -95.00000000000000000 ) ) ;
#4499 = CARTESIAN_POINT ( 'NONE',  ( 9.184850993605145972E-16, -49.99999999999997158, -97.09999999781504698 ) ) ;
#4500 = AXIS2_PLACEMENT_3D ( 'NONE', #2229, #6227, #6143 ) ;
#4501 = CARTESIAN_POINT ( 'NONE',  ( -22.03669253526174998, -40.34999999999999432, 4.057507815433014642 ) ) ;
#4502 = DIRECTION ( 'NONE',  ( 0.000000000000000000, 1.000000000000000000, -0.000000000000000000 ) ) ;
#4503 = CARTESIAN_POINT ( 'NONE',  ( 0.000000000000000000, 1.773042676681340968, -1.951563910473907981E-15 ) ) ;
#4504 = ADVANCED_FACE ( 'NONE', ( #6710 ), #532, .F. ) ;
#4505 = CARTESIAN_POINT ( 'NONE',  ( 0.000000000000000000, 80.00000000000002842, 0.000000000000000000 ) ) ;
#4506 = ORIENTED_EDGE ( 'NONE', *, *, #5477, .F. ) ;
#4507 = CARTESIAN_POINT ( 'NONE',  ( -23.71967171589458445, -49.74859572486944614, -6.359104887540838469 ) ) ;
#4508 = CARTESIAN_POINT ( 'NONE',  ( -21.53543802021056663, -33.90000000000000568, -4.312909747525783821 ) ) ;
#4509 = CARTESIAN_POINT ( 'NONE',  ( -38.38706344316003793, -43.70140427513058512, -1.382017864820032083 ) ) ;
#4510 = CARTESIAN_POINT ( 'NONE',  ( 2.071067811865474173, -39.99999999999997158, -96.04999999999999716 ) ) ;
#4511 = VECTOR ( 'NONE', #3624, 1000.000000000000000 ) ;
#4512 = CARTESIAN_POINT ( 'NONE',  ( 34.48171389889316885, -42.77717578641264140, 11.66923617342547992 ) ) ;
#4513 = CARTESIAN_POINT ( 'NONE',  ( -25.41550616830297571, -35.64859572486943051, 8.874878320068054549 ) ) ;
#4514 = CARTESIAN_POINT ( 'NONE',  ( -25.68709025247441602, -39.60000000000000853, -8.464561979789547053 ) ) ;
#4515 = CARTESIAN_POINT ( 'NONE',  ( -2.796473189345805913E-16, -40.43301269999997061, -99.64999999890751781 ) ) ;
#4516 = LINE ( 'NONE', #4033, #4424 ) ;
#4517 = CARTESIAN_POINT ( 'NONE',  ( 4.566987299999998307, -43.10829192115428299, -95.59999999890754907 ) ) ;
#4518 =( NAMED_UNIT ( * ) PLANE_ANGLE_UNIT ( ) SI_UNIT ( $, .RADIAN. ) );
#4519 = ORIENTED_EDGE ( 'NONE', *, *, #6729, .F. ) ;
#4520 = DIRECTION ( 'NONE',  ( 1.000000000000000000, 0.000000000000000000, 0.000000000000000000 ) ) ;
#4521 = ADVANCED_FACE ( 'NONE', ( #8041 ), #6054, .F. ) ;
#4522 = CARTESIAN_POINT ( 'NONE',  ( -28.61798213517984024, -47.79859572486944330, 8.387063443159973986 ) ) ;
#4523 = CARTESIAN_POINT ( 'NONE',  ( -25.63988726744978663, -32.60140427513057659, -8.440510857627391061 ) ) ;
#4524 = PRESENTATION_LAYER_ASSIGNMENT (  '', '', ( #8334 ) ) ;
#4525 = VERTEX_POINT ( 'NONE', #7288 ) ;
#4526 = ORIENTED_EDGE ( 'NONE', *, *, #130, .F. ) ;
#4527 = CARTESIAN_POINT ( 'NONE',  ( -20.12537475255788522, -33.05140427513057233, -1.507589171976365439 ) ) ;
#4528 = CARTESIAN_POINT ( 'NONE',  ( -34.87047186778190877, -46.14268964625814817, 11.51215629180721400 ) ) ;
#4529 = LINE ( 'NONE', #5810, #2476 ) ;
#4530 = PLANE ( 'NONE',  #5232 ) ;
#4531 = DIRECTION ( 'NONE',  ( -1.000000000000000000, -0.000000000000000000, -0.000000000000000000 ) ) ;
#4532 = DIRECTION ( 'NONE',  ( -0.000000000000000000, 1.000000000000000000, -0.000000000000000000 ) ) ;
#4533 = CARTESIAN_POINT ( 'NONE',  ( 4.999999999999998224, -42.92893218813448897, -97.75000000000001421 ) ) ;
#4534 = ORIENTED_EDGE ( 'NONE', *, *, #6083, .T. ) ;
#4535 =( REPRESENTATION_RELATIONSHIP ('NONE','NONE', #2265, #3450 ) REPRESENTATION_RELATIONSHIP_WITH_TRANSFORMATION ( #2751 )SHAPE_REPRESENTATION_RELATIONSHIP( ) );
#4536 = CARTESIAN_POINT ( 'NONE',  ( -21.17260567462091458, -40.05000000000001137, -1.398121909749242331 ) ) ;
#4537 = EDGE_LOOP ( 'NONE', ( #3475, #2135, #3550, #1501, #7473 ) ) ;
#4538 = CARTESIAN_POINT ( 'NONE',  ( -3.535533905932735532, -48.53553390593270933, -98.90000000000000568 ) ) ;
#4539 = VECTOR ( 'NONE', #7840, 1000.000000000000000 ) ;
#4540 = DIRECTION ( 'NONE',  ( 0.000000000000000000, 0.000000000000000000, 1.000000000000000000 ) ) ;
#4541 = CARTESIAN_POINT ( 'NONE',  ( -28.72263195913613387, -36.80140427513057944, 8.403638346957361449 ) ) ;
#4542 = EDGE_CURVE ( 'NONE', #2323, #4041, #1130, .T. ) ;
#4543 = AXIS2_PLACEMENT_3D ( 'NONE', #4259, #949, #5008 ) ;
#4544 = CARTESIAN_POINT ( 'NONE',  ( 5.000000000000000000, -47.07106781186545419, -96.94999999781504130 ) ) ;
#4545 = CARTESIAN_POINT ( 'NONE',  ( -22.42644454439892598, -33.90000000000000568, -3.858919247786222861 ) ) ;
#4546 = EDGE_CURVE ( 'NONE', #2752, #3764, #2410, .T. ) ;
#4547 = CARTESIAN_POINT ( 'NONE',  ( 30.00000000000001421, -49.99999999999997158, 12.49999999999995914 ) ) ;
#4548 = DIRECTION ( 'NONE',  ( 1.000000000000000000, 0.000000000000000000, 0.000000000000000000 ) ) ;
#4549 = CARTESIAN_POINT ( 'NONE',  ( 0.000000000000000000, 80.00000000000002842, 0.000000000000000000 ) ) ;
#4550 = VECTOR ( 'NONE', #5097, 1000.000000000000000 ) ;
#4551 = EDGE_LOOP ( 'NONE', ( #337, #8326, #414, #7732 ) ) ;
#4552 = CARTESIAN_POINT ( 'NONE',  ( -34.10713997105786888, -49.14859572486945183, -7.938018618334151455 ) ) ;
#4553 = CARTESIAN_POINT ( 'NONE',  ( -31.56260684030781505, -31.95000000000000639, 9.865911304835510265 ) ) ;
#4554 = CARTESIAN_POINT ( 'NONE',  ( -21.61293655684001536, -42.20140427513058512, 1.382017864820032971 ) ) ;
#4555 = ADVANCED_FACE ( 'NONE', ( #6050 ), #8659, .T. ) ;
#4556 = AXIS2_PLACEMENT_3D ( 'NONE', #8699, #6620, #7289 ) ;
#4557 = LINE ( 'NONE', #3287, #6147 ) ;
#4558 = DIRECTION ( 'NONE',  ( -0.000000000000000000, -1.000000000000000000, 0.000000000000000000 ) ) ;
#4559 = CARTESIAN_POINT ( 'NONE',  ( -23.24502507771338600, -38.49859572486943904, 6.680053920257780220 ) ) ;
#4560 = CARTESIAN_POINT ( 'NONE',  ( -37.06321265474346660, -38.25000000000001421, 7.063212654743582952 ) ) ;
#4561 = CARTESIAN_POINT ( 'NONE',  ( -41.99999999999996447, 48.00000000000002842, 22.00000000000000000 ) ) ;
#4562 = CARTESIAN_POINT ( 'NONE',  ( -30.00000000000002487, 0.000000000000000000, -26.00000000000000355 ) ) ;
#4563 = CARTESIAN_POINT ( 'NONE',  ( 1.891708078845682595, -40.43301269999998482, -98.89999999890751781 ) ) ;
#4564 = PRESENTATION_STYLE_ASSIGNMENT (( #7956 ) ) ;
#4565 = ORIENTED_EDGE ( 'NONE', *, *, #7287, .F. ) ;
#4566 = CARTESIAN_POINT ( 'NONE',  ( 42.00000000000000711, 48.00000000000002842, 23.64999999999992042 ) ) ;
#4567 = CARTESIAN_POINT ( 'NONE',  ( -28.49241082802385350, -31.44859572486944188, -9.874625247442173404 ) ) ;
#4568 = CARTESIAN_POINT ( 'NONE',  ( -28.38237549136062654, -29.45140427513057801, -9.857197362228843573 ) ) ;
#4569 = EDGE_CURVE ( 'NONE', #4798, #5904, #1286, .T. ) ;
#4570 = ORIENTED_EDGE ( 'NONE', *, *, #7226, .T. ) ;
#4571 = VERTEX_POINT ( 'NONE', #3986 ) ;
#4572 = CARTESIAN_POINT ( 'NONE',  ( -31.43380250590416125, -32.30140427513056522, -9.391326687552492558 ) ) ;
#4573 = EDGE_CURVE ( 'NONE', #1053, #8058, #1548, .T. ) ;
#4574 = DIRECTION ( 'NONE',  ( 0.000000000000000000, 0.000000000000000000, 1.000000000000000000 ) ) ;
#4575 = EDGE_CURVE ( 'NONE', #4984, #923, #6899, .T. ) ;
#4576 = CARTESIAN_POINT ( 'NONE',  ( -36.36396103067902175, -30.00000000000000711, -6.363961030678874309 ) ) ;
#4577 = CARTESIAN_POINT ( 'NONE',  ( -2.796473189345805913E-16, -40.43301269999997061, -100.4499999989075292 ) ) ;
#4578 = DIRECTION ( 'NONE',  ( 0.000000000000000000, 0.000000000000000000, -1.000000000000000000 ) ) ;
#4579 = ORIENTED_EDGE ( 'NONE', *, *, #6310, .T. ) ;
#4580 = CARTESIAN_POINT ( 'NONE',  ( -38.39535089505872634, -38.70000000000000284, -1.329692952841885267 ) ) ;
#4581 = EDGE_LOOP ( 'NONE', ( #4506, #3007 ) ) ;
#4582 = CARTESIAN_POINT ( 'NONE',  ( -4.999999999999997335, -47.07106781186546129, -97.35000000000000853 ) ) ;
#4583 = CARTESIAN_POINT ( 'NONE',  ( -34.53486167607238144, -48.15000000000001279, -8.900167166472096270 ) ) ;
#4584 = CARTESIAN_POINT ( 'NONE',  ( 4.566987300000000083, -46.89170807884565306, -98.09999999890752065 ) ) ;
#4585 = DIRECTION ( 'NONE',  ( 0.000000000000000000, 0.000000000000000000, 1.000000000000000000 ) ) ;
#4586 = TOROIDAL_SURFACE ( 'NONE', #8112, 2.000000000000000000, 1.000000000000000000 ) ;
#4587 = CARTESIAN_POINT ( 'NONE',  ( -31.27736804086391942, -35.30140427513057944, -8.403638346957361449 ) ) ;
#4588 = EDGE_CURVE ( 'NONE', #1009, #2150, #7603, .T. ) ;
#4589 = CARTESIAN_POINT ( 'NONE',  ( 3.535533905932736420, -41.46446609406723383, -96.89300000002185698 ) ) ;
#4590 = CARTESIAN_POINT ( 'NONE',  ( -23.68028341417693738, -33.75000000000000711, -6.319716585823200283 ) ) ;
#4591 = DIRECTION ( 'NONE',  ( 0.000000000000000000, 0.000000000000000000, 1.000000000000000000 ) ) ;
#4592 = TOROIDAL_SURFACE ( 'NONE', #7693, 2.000000000000000000, 1.000000000000000000 ) ;
#4593 = CARTESIAN_POINT ( 'NONE',  ( -37.06321265474346660, -50.24999999999999289, 7.063212654743582952 ) ) ;
#4594 = VERTEX_POINT ( 'NONE', #8354 ) ;
#4595 = CARTESIAN_POINT ( 'NONE',  ( -4.999999999999998224, -44.99999999999997158, -99.79999999999999716 ) ) ;
#4596 = AXIS2_PLACEMENT_3D ( 'NONE', #1482, #6249, #6946 ) ;
#4597 = CARTESIAN_POINT ( 'NONE',  ( -23.28248557872775137, -34.50000000000000000, 6.717514421272141156 ) ) ;
#4598 = CARTESIAN_POINT ( 'NONE',  ( -28.72263195913613387, -39.80140427513057944, 8.403638346957361449 ) ) ;
#4599 = CARTESIAN_POINT ( 'NONE',  ( -50.00000000000002842, -30.00000000000000000, 80.00000000000002842 ) ) ;
#4600 = AXIS2_PLACEMENT_3D ( 'NONE', #1279, #1239, #5959 ) ;
#4601 = LINE ( 'NONE', #7284, #4188 ) ;
#4602 = CARTESIAN_POINT ( 'NONE',  ( -28.49241082802385350, -34.44859572486944188, -9.874625247442173404 ) ) ;
#4603 = CARTESIAN_POINT ( 'NONE',  ( -22.93678734525658314, -42.75000000000001421, -7.063212654743582952 ) ) ;
#4604 = DIRECTION ( 'NONE',  ( -0.000000000000000000, -0.000000000000000000, 1.000000000000000000 ) ) ;
#4605 = CARTESIAN_POINT ( 'NONE',  ( -4.999999999999998224, -44.99999999999997158, -99.79999999999999716 ) ) ;
#4606 = CARTESIAN_POINT ( 'NONE',  ( -2.796473189345805913E-16, -40.43301269999997061, -98.84999999890752065 ) ) ;
#4607 = EDGE_LOOP ( 'NONE', ( #1809, #8701, #6628, #1725 ) ) ;
#4608 = CARTESIAN_POINT ( 'NONE',  ( -35.35889894354067309, 8.999999999999998224, -25.00000000000000000 ) ) ;
#4609 = CARTESIAN_POINT ( 'NONE',  ( -38.40363834695740053, -51.69859572486944188, -1.277368040863739118 ) ) ;
#4610 = CARTESIAN_POINT ( 'NONE',  ( -31.61762450863942320, -33.95140427513058512, 9.857197362228843573 ) ) ;
#4611 = VECTOR ( 'NONE', #6654, 1000.000000000000114 ) ;
#4612 = ORIENTED_EDGE ( 'NONE', *, *, #1988, .F. ) ;
#4613 = VERTEX_POINT ( 'NONE', #2977 ) ;
#4614 = CARTESIAN_POINT ( 'NONE',  ( -25.63988726744978663, -44.60140427513058370, -8.440510857627391061 ) ) ;
#4615 = DIRECTION ( 'NONE',  ( -1.000000000000000000, -0.000000000000000000, -0.000000000000000000 ) ) ;
#4616 = DIRECTION ( 'NONE',  ( 1.000000000000000000, 0.000000000000000000, 0.000000000000000000 ) ) ;
#4617 = CARTESIAN_POINT ( 'NONE',  ( 3.535533905932737309, -48.53553390593270933, -100.1999999978150555 ) ) ;
#4618 = DIRECTION ( 'NONE',  ( 0.000000000000000000, 0.000000000000000000, 1.000000000000000000 ) ) ;
#4619 = CARTESIAN_POINT ( 'NONE',  ( 3.535533905932736420, -41.46446609406723383, -98.50000000000000000 ) ) ;
#4620 = VERTEX_POINT ( 'NONE', #3593 ) ;
#4621 = CARTESIAN_POINT ( 'NONE',  ( -38.39535089505872634, -41.70000000000000995, -1.329692952841885267 ) ) ;
#4622 =( BOUNDED_CURVE ( )  B_SPLINE_CURVE ( 2, ( #1436, #3476, #6896, #3559, #6157, #6282, #6242, #2943, #241, #114, #4172, #2813, #5572, #4790, #1563, #1477, #7558, #201, #5484, #4963, #6984, #2904, #4258, #8193, #3643, #8237, #2282, #6197, #4131, #2151, #6941, #8320, #4213, #4838, #6853, #4920, #7600, #3601, #8364, #817, #3518, #5618, #160, #1520, #2195, #2856, #7474, #7646, #1610, #5531, #6323, #4299, #948, #286, #4880, #2988, #5662, #3853, #8486, #442, #7737, #1789, #3033, #1158, #5750, #8525, #3728, #7695, #5705, #4470, #5835, #6533, #2451, #8408, #5132, #4432, #1077, #987, #4389, #2491, #2328, #365, #482, #7779, #3074, #1656, #7824, #3197, #7115, #4347, #7156, #3771, #5880, #5172, #2373, #6491, #5006, #7027, #1749, #1116, #3686 ),
 .UNSPECIFIED., .F., .T. ) 
 B_SPLINE_CURVE_WITH_KNOTS ( ( 3, 2, 2, 2, 2, 2, 2, 2, 2, 2, 2, 2, 2, 2, 2, 2, 2, 2, 2, 2, 2, 2, 2, 2, 2, 2, 2, 2, 2, 2, 2, 2, 2, 2, 2, 2, 2, 2, 2, 2, 2, 2, 2, 2, 2, 2, 2, 2, 2, 2, 3 ),
 ( 0.000000000000000000, 0.01785714285714285615, 0.03571428571428571230, 0.05357142857142856845, 0.07142857142857142461, 0.08928571428571428770, 0.1071428571428571369, 0.1250000000000000000, 0.1428571428571428492, 0.1607142857142857262, 0.1785714285714285754, 0.1964285714285714246, 0.2142857142857142738, 0.2321428571428571508, 0.2500000000000000000, 0.2678571428571428492, 0.2857142857142856984, 0.3035714285714285476, 0.3214285714285714524, 0.3392857142857143016, 0.3571428571428571508, 0.3750000000000000000, 0.3928571428571428492, 0.4107142857142856984, 0.4285714285714285476, 0.4464285714285714524, 0.4642857142857143016, 0.4821428571428571508, 0.5000000000000000000, 0.5178571428571429047, 0.5357142857142856984, 0.5535714285714286031, 0.5714285714285713969, 0.5892857142857143016, 0.6071428571428570953, 0.6250000000000000000, 0.6428571428571429047, 0.6607142857142856984, 0.6785714285714286031, 0.6964285714285715079, 0.7142857142857143016, 0.7321428571428570953, 0.7500000000000000000, 0.7678571428571429047, 0.7857142857142856984, 0.8035714285714286031, 0.8214285714285713969, 0.8392857142857143016, 0.8571428571428570953, 0.8750000000000000000, 0.8928571428571429047 ),
 .UNSPECIFIED. ) 
 CURVE ( )  GEOMETRIC_REPRESENTATION_ITEM ( )  RATIONAL_B_SPLINE_CURVE ( ( 1.000000000000000000, 0.9238795325112867385, 1.000000000000000000, 0.9238795325112867385, 1.000000000000000000, 0.9238795325112867385, 1.000000000000000000, 0.9238795325112867385, 1.000000000000000000, 0.9238795325112867385, 1.000000000000000000, 0.9238795325112867385, 1.000000000000000000, 0.9238795325112867385, 1.000000000000000000, 0.9238795325112867385, 1.000000000000000000, 0.9238795325112867385, 1.000000000000000000, 0.9238795325112867385, 1.000000000000000000, 0.9238795325112867385, 1.000000000000000000, 0.9238795325112867385, 1.000000000000000000, 0.9238795325112867385, 1.000000000000000000, 0.9238795325112867385, 1.000000000000000000, 0.9238795325112867385, 1.000000000000000000, 0.9238795325112867385, 1.000000000000000000, 0.9238795325112867385, 1.000000000000000000, 0.9238795325112867385, 1.000000000000000000, 0.9238795325112867385, 1.000000000000000000, 0.9238795325112867385, 1.000000000000000000, 0.9238795325112867385, 1.000000000000000000, 0.9238795325112867385, 1.000000000000000000, 0.9238795325112867385, 1.000000000000000000, 0.9238795325112867385, 1.000000000000000000, 0.9238795325112867385, 1.000000000000000000, 0.9238795325112867385, 1.000000000000000000, 0.9238795325112867385, 1.000000000000000000, 0.9238795325112867385, 1.000000000000000000, 0.9238795325112867385, 1.000000000000000000, 0.9238795325112867385, 1.000000000000000000, 0.9238795325112867385, 1.000000000000000000, 0.9238795325112867385, 1.000000000000000000, 0.9238795325112867385, 1.000000000000000000, 0.9238795325112867385, 1.000000000000000000, 0.9238795325112867385, 1.000000000000000000, 0.9238795325112867385, 1.000000000000000000, 0.9238795325112867385, 1.000000000000000000, 0.9238795325112867385, 1.000000000000000000, 0.9238795325112867385, 1.000000000000000000, 0.9238795325112867385, 1.000000000000000000, 0.9238795325112867385, 1.000000000000000000, 0.9238795325112867385, 1.000000000000000000, 0.9238795325112867385, 1.000000000000000000, 0.9238795325112867385, 1.000000000000000000, 0.9238795325112867385, 1.000000000000000000, 0.9238795325112867385, 1.000000000000000000, 0.9238795325112867385, 1.000000000000000000, 0.9238795325112867385, 1.000000000000000000, 0.9238795325112867385, 1.000000000000000000, 0.9238795325112867385, 1.000000000000000000 ) ) 
 REPRESENTATION_ITEM ( '' )  );
#4623 = VERTEX_POINT ( 'NONE', #104 ) ;
#4624 = CARTESIAN_POINT ( 'NONE',  ( -30.00000000000000000, 60.00000000000002842, -12.49999999999998046 ) ) ;
#4625 = CARTESIAN_POINT ( 'NONE',  ( -2.071067811865475061, -39.99999999999997158, -95.84999999781503277 ) ) ;
#4626 = CARTESIAN_POINT ( 'NONE',  ( -28.51387258211773812, -46.80000000000001137, 9.383039235653802379 ) ) ;
#4627 = CARTESIAN_POINT ( 'NONE',  ( -3.229347689422840784, -41.77065231057713390, -99.34999999890753486 ) ) ;
#4628 = DIRECTION ( 'NONE',  ( -0.000000000000000000, 1.000000000000000000, -0.000000000000000000 ) ) ;
#4629 = CARTESIAN_POINT ( 'NONE',  ( -22.40239342223677355, -29.90140427513058796, -3.811716262761597473 ) ) ;
#4630 = CARTESIAN_POINT ( 'NONE',  ( -3.061616997868382155E-16, -39.99999999999997158, -97.59300000002185982 ) ) ;
#4631 = CARTESIAN_POINT ( 'NONE',  ( -22.42644454439892598, -36.90000000000000568, -3.858919247786222861 ) ) ;
#4632 = DIRECTION ( 'NONE',  ( -0.000000000000000000, 1.000000000000000000, -0.000000000000000000 ) ) ;
#4633 = FACE_OUTER_BOUND ( 'NONE', #7219, .T. ) ;
#4634 = DIRECTION ( 'NONE',  ( 1.000000000000000000, 0.000000000000000000, 0.000000000000000000 ) ) ;
#4635 = VERTEX_POINT ( 'NONE', #8310 ) ;
#4636 = CARTESIAN_POINT ( 'NONE',  ( 7.499999999999999112, -44.99999999999997158, -105.0000000000000142 ) ) ;
#4637 = CARTESIAN_POINT ( 'NONE',  ( -21.09983283352784156, -43.35000000000000853, 4.534861676072186043 ) ) ;
#4638 = CARTESIAN_POINT ( 'NONE',  ( -33.90612223281073057, -46.10140427513058370, 7.549504333439023718 ) ) ;
#4639 = VECTOR ( 'NONE', #3064, 1000.000000000000000 ) ;
#4640 = DIRECTION ( 'NONE',  ( 0.000000000000000000, 0.000000000000000000, 1.000000000000000000 ) ) ;
#4641 = LINE ( 'NONE', #2668, #8130 ) ;
#4642 = CARTESIAN_POINT ( 'NONE',  ( -21.55948914237271907, -37.89859572486944472, -4.360112732550413206 ) ) ;
#4643 = CARTESIAN_POINT ( 'NONE',  ( -33.35889894354067309, 8.000000000000000000, 124.0000000000000000 ) ) ;
#4644 = ADVANCED_BREP_SHAPE_REPRESENTATION ( '', ( #2959, #2554 ), #7620 ) ;
#4645 = DIRECTION ( 'NONE',  ( -0.000000000000000000, 1.000000000000000000, -0.000000000000000000 ) ) ;
#4646 = CARTESIAN_POINT ( 'NONE',  ( 3.229347689422841228, -48.22934768942280925, -99.94999999890752918 ) ) ;
#4647 = AXIS2_PLACEMENT_3D ( 'NONE', #231, #3548, #6800 ) ;
#4648 = VERTEX_POINT ( 'NONE', #3509 ) ;
#4649 = DIRECTION ( 'NONE',  ( 0.000000000000000000, 1.000000000000000000, 0.000000000000000000 ) ) ;
#4650 = CARTESIAN_POINT ( 'NONE',  ( -38.81868038277247734, -33.54859572486944330, 1.453139578080855365 ) ) ;
#4651 = CARTESIAN_POINT ( 'NONE',  ( -21.55948914237271907, -31.89859572486943762, -4.360112732550413206 ) ) ;
#4652 = CARTESIAN_POINT ( 'NONE',  ( -23.31994607974211675, -39.50140427513058228, 6.754974922286503869 ) ) ;
#4653 = AXIS2_PLACEMENT_3D ( 'NONE', #4495, #4628, #1142 ) ;
#4654 = ORIENTED_EDGE ( 'NONE', *, *, #4721, .F. ) ;
#4655 = ORIENTED_EDGE ( 'NONE', *, *, #7880, .F. ) ;
#4656 = CARTESIAN_POINT ( 'NONE',  ( -20.62524821624488069, -48.20140427513058512, 1.538452329860250378 ) ) ;
#4657 = DIRECTION ( 'NONE',  ( -0.000000000000000000, -0.000000000000000000, -1.000000000000000000 ) ) ;
#4658 = CARTESIAN_POINT ( 'NONE',  ( 3.535533905932736420, -41.46446609406723383, -99.99999999781503845 ) ) ;
#4659 = CARTESIAN_POINT ( 'NONE',  ( -2.071067811865475061, -39.99999999999997158, -95.14999999999999147 ) ) ;
#4660 = CARTESIAN_POINT ( 'NONE',  ( 4.999999999999998224, -42.92893218813448897, -98.54999999999999716 ) ) ;
#4661 = VERTEX_POINT ( 'NONE', #6272 ) ;
#4662 = AXIS2_PLACEMENT_3D ( 'NONE', #8473, #4540, #1775 ) ;
#4663 = CARTESIAN_POINT ( 'NONE',  ( -28.60187809025093841, -39.45000000000000995, -8.827394325379140483 ) ) ;
#4664 = EDGE_CURVE ( 'NONE', #4613, #5875, #6606, .T. ) ;
#4665 = CYLINDRICAL_SURFACE ( 'NONE', #3973, 3.500000000000000000 ) ;
#4666 = EDGE_LOOP ( 'NONE', ( #6042, #942, #22 ) ) ;
#4667 = CARTESIAN_POINT ( 'NONE',  ( 3.229347689422841228, -48.22934768942280925, -99.14999999890751781 ) ) ;
#4668 = EDGE_CURVE ( 'NONE', #4620, #799, #4346, .T. ) ;
#4669 = CARTESIAN_POINT ( 'NONE',  ( -2.071067811865475505, -49.99999999999996447, -99.64999999999999147 ) ) ;
#4670 = CARTESIAN_POINT ( 'NONE',  ( -22.93678734525658314, -48.75000000000001421, -7.063212654743582952 ) ) ;
#4671 = CARTESIAN_POINT ( 'NONE',  ( -4.566987299999998307, -44.99999999999997158, -97.64999999890753202 ) ) ;
#4672 = SURFACE_STYLE_FILL_AREA ( #4148 ) ;
#4673 = CARTESIAN_POINT ( 'NONE',  ( -22.06198138166579170, -30.35140427513058015, 4.107139971057695682 ) ) ;
#4674 =( BOUNDED_CURVE ( )  B_SPLINE_CURVE ( 2, ( #3202, #5885, #6097, #6667, #5925, #1331, #5966, #56, #622 ),
 .UNSPECIFIED., .F., .T. ) 
 B_SPLINE_CURVE_WITH_KNOTS ( ( 3, 2, 2, 2, 3 ),
 ( 0.5714285714285713969, 0.5892857142857143016, 0.6071428571428570953, 0.6250000000000000000, 0.6428571428571429047 ),
 .UNSPECIFIED. ) 
 CURVE ( )  GEOMETRIC_REPRESENTATION_ITEM ( )  RATIONAL_B_SPLINE_CURVE ( ( 1.000000000000000000, 0.9238795325112867385, 1.000000000000000000, 0.9238795325112867385, 1.000000000000000000, 0.9238795325112867385, 1.000000000000000000, 0.9238795325112867385, 1.000000000000000000 ) ) 
 REPRESENTATION_ITEM ( '' )  );
#4675 = EDGE_CURVE ( 'NONE', #4683, #1297, #4119, .T. ) ;
#4676 = CARTESIAN_POINT ( 'NONE',  ( 4.999999999999998224, -42.92893218813448897, -96.14300000002184277 ) ) ;
#4677 = CIRCLE ( 'NONE', #5806, 7.499999999999999112 ) ;
#4678 = CARTESIAN_POINT ( 'NONE',  ( -28.67030704715798350, -31.80000000000000782, 8.395350895058669494 ) ) ;
#4679 = EDGE_CURVE ( 'NONE', #7382, #5578, #143, .T. ) ;
#4680 = CYLINDRICAL_SURFACE ( 'NONE', #1508, 12.00000000000004263 ) ;
#4681 = DIRECTION ( 'NONE',  ( -0.000000000000000000, -0.000000000000000000, 1.000000000000000000 ) ) ;
#4682 = DIRECTION ( 'NONE',  ( 1.000000000000000000, 0.000000000000000000, 0.000000000000000000 ) ) ;
#4683 = VERTEX_POINT ( 'NONE', #2934 ) ;
#4684 = CARTESIAN_POINT ( 'NONE',  ( 4.999999999999998224, -44.99999999999997158, -99.40000000000000568 ) ) ;
#4685 = AXIS2_PLACEMENT_3D ( 'NONE', #7276, #3889, #4548 ) ;
#4686 = CARTESIAN_POINT ( 'NONE',  ( -34.53486167607238144, -45.14999999999999858, -8.900167166472096270 ) ) ;
#4687 = CARTESIAN_POINT ( 'NONE',  ( -22.40239342223677355, -47.90140427513058086, -3.811716262761597473 ) ) ;
#4688 = VECTOR ( 'NONE', #4446, 1000.000000000000114 ) ;
#4689 = EDGE_CURVE ( 'NONE', #5629, #8625, #7750, .T. ) ;
#4690 = CARTESIAN_POINT ( 'NONE',  ( -41.99999999999996447, 60.00000000000002842, 22.00000000000000000 ) ) ;
#4691 = DIRECTION ( 'NONE',  ( -0.000000000000000000, -0.000000000000000000, -1.000000000000000000 ) ) ;
#4692 = CARTESIAN_POINT ( 'NONE',  ( -28.49241082802385350, -49.44859572486943478, -9.874625247442173404 ) ) ;
#4693 = LINE ( 'NONE', #5429, #7033 ) ;
#4694 = AXIS2_PLACEMENT_3D ( 'NONE', #5485, #3560, #6244 ) ;
#4695 = CARTESIAN_POINT ( 'NONE',  ( 0.000000000000000000, 0.000000000000000000, 125.0000000000000000 ) ) ;
#4696 = CARTESIAN_POINT ( 'NONE',  ( -4.566987299999998307, -43.10829192115428299, -96.09999999890752065 ) ) ;
#4697 = VERTEX_POINT ( 'NONE', #894 ) ;
#4698 = CARTESIAN_POINT ( 'NONE',  ( 2.000000000000000000, 0.8865213383406717051, 1.535499999999999199 ) ) ;
#4699 = CARTESIAN_POINT ( 'NONE',  ( -36.04786814110010340, -33.99859572486943904, -5.972947139071243861 ) ) ;
#4700 = CARTESIAN_POINT ( 'NONE',  ( -38.44051085762733777, -42.39859572486944472, 4.360112732550414982 ) ) ;
#4701 = CARTESIAN_POINT ( 'NONE',  ( -36.68005392025794009, -44.00140427513057517, -6.754974922286504757 ) ) ;
#4702 = ORIENTED_EDGE ( 'NONE', *, *, #4106, .T. ) ;
#4703 = ORIENTED_EDGE ( 'NONE', *, *, #7374, .T. ) ;
#4704 = CARTESIAN_POINT ( 'NONE',  ( -23.31994607974211675, -45.50140427513058228, 6.754974922286503869 ) ) ;
#4705 = EDGE_CURVE ( 'NONE', #2692, #7480, #423, .T. ) ;
#4706 = FILL_AREA_STYLE ('',( #2110 ) ) ;
#4707 = CARTESIAN_POINT ( 'NONE',  ( -33.35889894354067309, 8.000000000000000000, -25.00000000000000000 ) ) ;
#4708 = CARTESIAN_POINT ( 'NONE',  ( -3.535533905932736864, -41.46446609406723383, -98.19999999781505551 ) ) ;
#4709 = CARTESIAN_POINT ( 'NONE',  ( 33.05403370888239323, -48.97208017019577397, 12.12430375744700406 ) ) ;
#4710 = CARTESIAN_POINT ( 'NONE',  ( 3.535533905932737309, -48.53553390593270933, -98.70000000000000284 ) ) ;
#4711 = VECTOR ( 'NONE', #623, 1000.000000000000000 ) ;
#4712 = ORIENTED_EDGE ( 'NONE', *, *, #5404, .T. ) ;
#4713 = CARTESIAN_POINT ( 'NONE',  ( -28.67030704715798350, -49.80000000000001137, 8.395350895058669494 ) ) ;
#4714 = CARTESIAN_POINT ( 'NONE',  ( -21.09983283352784156, -37.35000000000000853, 4.534861676072186043 ) ) ;
#4715 = ORIENTED_EDGE ( 'NONE', *, *, #4664, .T. ) ;
#4716 = CARTESIAN_POINT ( 'NONE',  ( 3.229347689422839895, -41.77065231057713390, -96.54999999890752349 ) ) ;
#4717 = CARTESIAN_POINT ( 'NONE',  ( -3.535533905932736864, -41.46446609406723383, -97.39999999781504414 ) ) ;
#4718 = CARTESIAN_POINT ( 'NONE',  ( -34.31290974752564438, -41.10000000000000142, 8.464561979789547053 ) ) ;
#4719 = CARTESIAN_POINT ( 'NONE',  ( 4.566987299999998307, -43.10829192115428299, -98.79999999890753770 ) ) ;
#4720 = CARTESIAN_POINT ( 'NONE',  ( -28.54686042191934092, -32.45140427513058512, -8.818680382772479120 ) ) ;
#4721 = EDGE_CURVE ( 'NONE', #8337, #6952, #5653, .T. ) ;
#4722 = CARTESIAN_POINT ( 'NONE',  ( 3.535533905932736420, -41.46446609406723383, -96.09300000002185982 ) ) ;
#4723 = VECTOR ( 'NONE', #6997, 1000.000000000000000 ) ;
#4724 = CARTESIAN_POINT ( 'NONE',  ( -22.42644454439892598, -42.90000000000000568, -3.858919247786222861 ) ) ;
#4725 = FACE_OUTER_BOUND ( 'NONE', #166, .T. ) ;
#4726 = CARTESIAN_POINT ( 'NONE',  ( -4.999999999999998224, -44.99999999999997158, -95.69999999781504130 ) ) ;
#4727 = PRODUCT_CONTEXT ( 'NONE', #7853, 'mechanical' ) ;
#4728 = ORIENTED_EDGE ( 'NONE', *, *, #1642, .F. ) ;
#4729 = CARTESIAN_POINT ( 'NONE',  ( -20.00000000000002487, 0.000000000000000000, -26.00000000000000355 ) ) ;
#4730 = CARTESIAN_POINT ( 'NONE',  ( -21.09983283352784156, -46.34999999999998721, 4.534861676072186043 ) ) ;
#4731 = CARTESIAN_POINT ( 'NONE',  ( -38.38706344316003793, -46.70140427513057801, -1.382017864820032083 ) ) ;
#4732 = AXIS2_PLACEMENT_3D ( 'NONE', #7926, #3917, #4578 ) ;
#4733 = CARTESIAN_POINT ( 'NONE',  ( 4.999999999999994671, -42.92893218813449607, -96.95000000000000284 ) ) ;
#4734 = CARTESIAN_POINT ( 'NONE',  ( -4.999999999999998224, -44.99999999999997158, -95.00000000000000000 ) ) ;
#4735 = CARTESIAN_POINT ( 'NONE',  ( -20.60867331244750034, -50.19859572486944188, 1.433802505903951419 ) ) ;
#4736 = EDGE_CURVE ( 'NONE', #7915, #8652, #416, .T. ) ;
#4737 = CARTESIAN_POINT ( 'NONE',  ( 2.000000000000000000, -0.8865213383406692627, 1.535500000000001641 ) ) ;
#4738 = CARTESIAN_POINT ( 'NONE',  ( -39.86591130483550671, -32.55000000000000426, 1.562606840307984690 ) ) ;
#4739 = CARTESIAN_POINT ( 'NONE',  ( 8.389419568037416259E-16, -49.56698729999997255, -96.64999999890753202 ) ) ;
#4740 = ORIENTED_EDGE ( 'NONE', *, *, #7645, .T. ) ;
#4741 = CARTESIAN_POINT ( 'NONE',  ( -26.14108075221394856, -45.60000000000000853, -7.573555455601170827 ) ) ;
#4742 = CARTESIAN_POINT ( 'NONE',  ( -25.41550616830297571, -35.64859572486943051, 8.874878320068054549 ) ) ;
#4743 = CARTESIAN_POINT ( 'NONE',  ( -23.31994607974211675, -45.50140427513058228, 6.754974922286503869 ) ) ;
#4744 = ORIENTED_EDGE ( 'NONE', *, *, #2472, .F. ) ;
#4745 = ORIENTED_EDGE ( 'NONE', *, *, #7374, .F. ) ;
#4746 = CARTESIAN_POINT ( 'NONE',  ( -28.38237549136062654, -41.45140427513058512, -9.857197362228843573 ) ) ;
#4747 = LINE ( 'NONE', #3303, #3285 ) ;
#4748 = DIRECTION ( 'NONE',  ( 0.000000000000000000, 0.000000000000000000, 1.000000000000000000 ) ) ;
#4749 = CARTESIAN_POINT ( 'NONE',  ( 9.184850993605145972E-16, -49.99999999999997158, -98.69999999781505551 ) ) ;
#4750 = CARTESIAN_POINT ( 'NONE',  ( 4.999999999999998224, -44.99999999999997158, -96.20000000000000284 ) ) ;
#4751 = CARTESIAN_POINT ( 'NONE',  ( -50.00000000000002842, -30.00000000000000000, 80.00000000000002842 ) ) ;
#4752 = AXIS2_PLACEMENT_3D ( 'NONE', #1930, #4657, #1345 ) ;
#4753 = ORIENTED_EDGE ( 'NONE', *, *, #4849, .F. ) ;
#4754 = VECTOR ( 'NONE', #4632, 1000.000000000000000 ) ;
#4755 = CARTESIAN_POINT ( 'NONE',  ( -34.10713997105786888, -34.14859572486943051, -7.938018618334151455 ) ) ;
#4756 = CARTESIAN_POINT ( 'NONE',  ( -38.46456197978948666, -38.40000000000000568, 4.312909747525784709 ) ) ;
#4757 = EDGE_CURVE ( 'NONE', #2964, #4999, #3464, .T. ) ;
#4758 = ORIENTED_EDGE ( 'NONE', *, *, #5404, .F. ) ;
#4759 = ORIENTED_EDGE ( 'NONE', *, *, #7035, .F. ) ;
#4760 = CARTESIAN_POINT ( 'NONE',  ( -4.566987299999998307, -44.99999999999997158, -97.04999999890752349 ) ) ;
#4761 = CARTESIAN_POINT ( 'NONE',  ( 2.071067811865477282, -49.99999999999996447, -97.84999999781504698 ) ) ;
#4762 = CARTESIAN_POINT ( 'NONE',  ( -31.48612741788231517, -45.30000000000000426, -9.383039235653804155 ) ) ;
#4763 = AXIS2_PLACEMENT_3D ( 'NONE', #1779, #7854, #6523 ) ;
#4764 = CARTESIAN_POINT ( 'NONE',  ( 1.891708078845685481, -49.56698729999997255, -98.99999999890752633 ) ) ;
#4765 = FACE_OUTER_BOUND ( 'NONE', #4450, .T. ) ;
#4766 = CARTESIAN_POINT ( 'NONE',  ( -31.27736804086391942, -44.30140427513057944, -8.403638346957361449 ) ) ;
#4767 = CARTESIAN_POINT ( 'NONE',  ( 9.184850993605145972E-16, -49.99999999999997158, -96.39300000002185698 ) ) ;
#4768 = CARTESIAN_POINT ( 'NONE',  ( -34.05750781543319050, -45.15000000000000568, -7.963307464738194952 ) ) ;
#4769 = CARTESIAN_POINT ( 'NONE',  ( 26.94219849796044031, -48.96939036817694557, 12.12340239416034748 ) ) ;
#4770 = EDGE_CURVE ( 'NONE', #3552, #3394, #6230, .T. ) ;
#4771 = CARTESIAN_POINT ( 'NONE',  ( 4.999999999999998224, -44.99999999999997158, -96.09999999781504698 ) ) ;
#4772 = ORIENTED_EDGE ( 'NONE', *, *, #6650, .F. ) ;
#4773 = CARTESIAN_POINT ( 'NONE',  ( -2.071067811865475505, -49.99999999999997158, -99.65000000000000568 ) ) ;
#4774 = CARTESIAN_POINT ( 'NONE',  ( -39.38303923565386100, -47.70000000000000284, -1.486127417882099788 ) ) ;
#4775 = CARTESIAN_POINT ( 'NONE',  ( -37.96330746473829976, -32.85000000000000853, -4.057507815433013754 ) ) ;
#4776 = CARTESIAN_POINT ( 'NONE',  ( -27.48070537354846365, -40.66893875716694140, 12.24660140962718735 ) ) ;
#4777 = LINE ( 'NONE', #8178, #2263 ) ;
#4778 = CARTESIAN_POINT ( 'NONE',  ( -39.39132668755255651, -48.69859572486944188, -1.433802505903950308 ) ) ;
#4779 = EDGE_CURVE ( 'NONE', #196, #2012, #8181, .T. ) ;
#4780 = CARTESIAN_POINT ( 'NONE',  ( -36.36396103067902175, -51.00000000000000711, -6.363961030678874309 ) ) ;
#4781 = CARTESIAN_POINT ( 'NONE',  ( -38.46456197978948666, -32.40000000000000568, 4.312909747525784709 ) ) ;
#4782 = SURFACE_STYLE_FILL_AREA ( #4827 ) ;
#4783 = ORIENTED_EDGE ( 'NONE', *, *, #1008, .T. ) ;
#4784 = DIRECTION ( 'NONE',  ( 1.000000000000000000, 0.000000000000000000, 0.000000000000000000 ) ) ;
#4785 = CARTESIAN_POINT ( 'NONE',  ( -37.57355545560112375, -47.40000000000001279, 3.858919247786223305 ) ) ;
#4786 = CARTESIAN_POINT ( 'NONE',  ( -37.02382435302582309, -42.24859572486943904, 7.102600956461226467 ) ) ;
#4787 = CARTESIAN_POINT ( 'NONE',  ( -20.12537475255788522, -42.05140427513057944, -1.507589171976365439 ) ) ;
#4788 = ORIENTED_EDGE ( 'NONE', *, *, #7138, .T. ) ;
#4789 = ORIENTED_EDGE ( 'NONE', *, *, #6666, .T. ) ;
#4790 = CARTESIAN_POINT ( 'NONE',  ( -1.891708078845683705, -49.56698729999997255, -95.89999999890753202 ) ) ;
#4791 = CARTESIAN_POINT ( 'NONE',  ( -2.796473189345805913E-16, -40.43301269999997061, -100.2499999989075263 ) ) ;
#4792 = DIRECTION ( 'NONE',  ( 0.000000000000000000, 0.000000000000000000, 1.000000000000000000 ) ) ;
#4793 = CIRCLE ( 'NONE', #4088, 2.099999999999997868 ) ;
#4794 = CARTESIAN_POINT ( 'NONE',  ( 8.389419568037416259E-16, -49.56698729999997255, -96.04999999890752349 ) ) ;
#4795 = DIRECTION ( 'NONE',  ( 0.000000000000000000, 0.000000000000000000, 1.000000000000000000 ) ) ;
#4796 = FACE_BOUND ( 'NONE', #3868, .T. ) ;
#4797 = EDGE_CURVE ( 'NONE', #6586, #7878, #5341, .T. ) ;
#4798 = VERTEX_POINT ( 'NONE', #848 ) ;
#4799 = CARTESIAN_POINT ( 'NONE',  ( -37.57355545560112375, -50.40000000000000568, 3.858919247786223305 ) ) ;
#4800 = CARTESIAN_POINT ( 'NONE',  ( -34.53486167607238144, -39.14999999999999147, -8.900167166472096270 ) ) ;
#4801 = EDGE_LOOP ( 'NONE', ( #3486, #725, #586, #2768 ) ) ;
#4802 = SURFACE_STYLE_USAGE ( .BOTH. , #212 ) ;
#4803 = CARTESIAN_POINT ( 'NONE',  ( -1.891708078845683039, -40.43301269999998482, -97.19999999890751496 ) ) ;
#4804 = CARTESIAN_POINT ( 'NONE',  ( -4.999999999999998224, -46.91341716182541433, -95.65380602118948161 ) ) ;
#4805 = AXIS2_PLACEMENT_3D ( 'NONE', #313, #3014, #8391 ) ;
#4806 = CARTESIAN_POINT ( 'NONE',  ( -34.31290974752564438, -50.10000000000000853, 8.464561979789547053 ) ) ;
#4807 = CARTESIAN_POINT ( 'NONE',  ( 1.891708078845682595, -40.43301269999998482, -97.09999999890753486 ) ) ;
#4808 = DIRECTION ( 'NONE',  ( 1.000000000000000000, 0.000000000000000000, 0.000000000000000000 ) ) ;
#4809 = CARTESIAN_POINT ( 'NONE',  ( -37.59760657776328685, -43.40140427513058796, 3.811716262761598362 ) ) ;
#4810 =( GEOMETRIC_REPRESENTATION_CONTEXT ( 3 ) GLOBAL_UNCERTAINTY_ASSIGNED_CONTEXT ( ( #5706 ) ) GLOBAL_UNIT_ASSIGNED_CONTEXT ( ( #3423, #763, #7508 ) ) REPRESENTATION_CONTEXT ( 'NONE', 'WORKASPACE' ) );
#4811 = CARTESIAN_POINT ( 'NONE',  ( 4.999999999999998224, -44.99999999999997158, -98.59300000002185982 ) ) ;
#4812 = CARTESIAN_POINT ( 'NONE',  ( -38.39535089505872634, -41.70000000000000995, -1.329692952841885267 ) ) ;
#4813 = CARTESIAN_POINT ( 'NONE',  ( -3.229347689422839451, -48.22934768942280925, -97.54999999890752349 ) ) ;
#4814 = LINE ( 'NONE', #2882, #2744 ) ;
#4815 = ORIENTED_EDGE ( 'NONE', *, *, #1396, .T. ) ;
#4816 = DIRECTION ( 'NONE',  ( -1.000000000000000000, -0.000000000000000000, -0.000000000000000000 ) ) ;
#4817 = CARTESIAN_POINT ( 'NONE',  ( -25.46513832392765408, -49.64999999999999147, 8.900167166472096270 ) ) ;
#4818 = EDGE_CURVE ( 'NONE', #3280, #5819, #4939, .T. ) ;
#4819 = CARTESIAN_POINT ( 'NONE',  ( -25.99212434019154472, -45.65140427513058086, 7.988596311142242890 ) ) ;
#4820 = AXIS2_PLACEMENT_3D ( 'NONE', #4707, #5311, #25 ) ;
#4821 = AXIS2_PLACEMENT_3D ( 'NONE', #140, #4284, #4241 ) ;
#4822 = DIRECTION ( 'NONE',  ( -0.000000000000000000, -0.000000000000000000, -1.000000000000000000 ) ) ;
#4823 = CARTESIAN_POINT ( 'NONE',  ( -41.99999999999996447, 48.00000000000002842, 22.00000000000000000 ) ) ;
#4824 = CARTESIAN_POINT ( 'NONE',  ( -25.73429323749904185, -49.59859572486944046, -8.488613101951701267 ) ) ;
#4825 = CARTESIAN_POINT ( 'NONE',  ( 5.000000000000000000, -47.07106781186545419, -97.85000000000003695 ) ) ;
#4826 = CARTESIAN_POINT ( 'NONE',  ( -36.71751442127229836, -30.00000000000000711, -6.717514421272142044 ) ) ;
#4828 = AXIS2_PLACEMENT_3D ( 'NONE', #2817, #6248, #8154 ) ;
#4827 = FILL_AREA_STYLE ('',( #2099 ) ) ;
#4829 = VERTEX_POINT ( 'NONE', #8399 ) ;
#4830 = DIRECTION ( 'NONE',  ( 0.000000000000000000, 0.000000000000000000, -1.000000000000000000 ) ) ;
#4831 = ORIENTED_EDGE ( 'NONE', *, *, #4194, .T. ) ;
#4832 = CONICAL_SURFACE ( 'NONE', #5593, 12.49999999999997335, 1.029744258676651869 ) ;
#4833 = CARTESIAN_POINT ( 'NONE',  ( -37.96330746473829976, -50.84999999999999432, -4.057507815433013754 ) ) ;
#4834 = CARTESIAN_POINT ( 'NONE',  ( -34.26570676250101855, -42.09859572486944046, 8.488613101951703044 ) ) ;
#4835 = CARTESIAN_POINT ( 'NONE',  ( -28.38237549136062654, -41.45140427513058512, -9.857197362228843573 ) ) ;
#4836 = EDGE_CURVE ( 'NONE', #5393, #8009, #474, .T. ) ;
#4837 = ORIENTED_EDGE ( 'NONE', *, *, #2963, .T. ) ;
#4838 = CARTESIAN_POINT ( 'NONE',  ( -4.566987299999998307, -43.10829192115428299, -96.89999999890753202 ) ) ;
#4839 = CARTESIAN_POINT ( 'NONE',  ( -49.99999999999997158, 60.00000000000002842, -30.00000000000000000 ) ) ;
#4840 = CARTESIAN_POINT ( 'NONE',  ( -34.99999999999997868, -44.66998333124467280, 11.45643923738958847 ) ) ;
#4841 = CARTESIAN_POINT ( 'NONE',  ( -1.891708078845683039, -40.43301269999998482, -96.39999999890753202 ) ) ;
#4842 = DIRECTION ( 'NONE',  ( 1.000000000000000000, 0.000000000000000000, 0.000000000000000000 ) ) ;
#4843 = FACE_BOUND ( 'NONE', #3513, .T. ) ;
#4844 = ORIENTED_EDGE ( 'NONE', *, *, #4199, .F. ) ;
#4845 = EDGE_CURVE ( 'NONE', #8009, #4594, #3675, .T. ) ;
#4846 = CARTESIAN_POINT ( 'NONE',  ( -31.34310424141748896, -35.94859572486944188, 8.836108267985801845 ) ) ;
#4847 = CARTESIAN_POINT ( 'NONE',  ( -34.31290974752564438, -35.10000000000000853, 8.464561979789547053 ) ) ;
#4848 = ORIENTED_EDGE ( 'NONE', *, *, #4949, .T. ) ;
#4849 = EDGE_CURVE ( 'NONE', #2769, #5614, #3025, .T. ) ;
#4850 = CARTESIAN_POINT ( 'NONE',  ( -22.93678734525658314, -48.75000000000001421, -7.063212654743582952 ) ) ;
#4851 = LINE ( 'NONE', #871, #7864 ) ;
#4852 = CARTESIAN_POINT ( 'NONE',  ( -3.229347689422839451, -48.22934768942280925, -97.74999999890751212 ) ) ;
#4853 = CARTESIAN_POINT ( 'NONE',  ( 2.000000000000000000, -0.8865213383406692627, 1.535500000000001641 ) ) ;
#4854 = DIRECTION ( 'NONE',  ( 1.000000000000000000, 0.000000000000000000, 0.000000000000000000 ) ) ;
#4855 = CARTESIAN_POINT ( 'NONE',  ( -4.566987299999998307, -44.99999999999997158, -99.24999999890752633 ) ) ;
#4856 = ADVANCED_FACE ( 'NONE', ( #5744 ), #383, .F. ) ;
#4857 = CARTESIAN_POINT ( 'NONE',  ( -21.16389173201424612, -42.05140427513057944, -1.343104241417630185 ) ) ;
#4858 = CARTESIAN_POINT ( 'NONE',  ( -2.071067811865475061, -39.99999999999997158, -99.94300000002185413 ) ) ;
#4859 = UNCERTAINTY_MEASURE_WITH_UNIT (LENGTH_MEASURE( 1.000000000000000082E-05 ), #372, 'distance_accuracy_value', 'NONE');
#4860 = CARTESIAN_POINT ( 'NONE',  ( -33.35889894354067309, 8.000000000000000000, 124.0000000000000000 ) ) ;
#4861 = CARTESIAN_POINT ( 'NONE',  ( -38.82739432537914581, -41.55000000000000426, 1.398121909749243663 ) ) ;
#4862 = FACE_OUTER_BOUND ( 'NONE', #6947, .T. ) ;
#4863 = SHAPE_DEFINITION_REPRESENTATION ( #5709, #6809 ) ;
#4864 = ORIENTED_EDGE ( 'NONE', *, *, #6003, .F. ) ;
#4865 = SURFACE_STYLE_FILL_AREA ( #6308 ) ;
#4866 = LINE ( 'NONE', #5513, #5382 ) ;
#4867 = CARTESIAN_POINT ( 'NONE',  ( -28.60187809025093841, -39.45000000000000995, -8.827394325379140483 ) ) ;
#4868 = EDGE_CURVE ( 'NONE', #1263, #3680, #7017, .T. ) ;
#4869 = CARTESIAN_POINT ( 'NONE',  ( -29.17564914869307202, -40.06565635038682416, 12.47384660903968623 ) ) ;
#4870 = DIRECTION ( 'NONE',  ( -1.000000000000000000, -0.000000000000000000, -0.000000000000000000 ) ) ;
#4871 = CARTESIAN_POINT ( 'NONE',  ( -39.39132668755255651, -51.69859572486944188, -1.433802505903950308 ) ) ;
#4872 = CARTESIAN_POINT ( 'NONE',  ( -4.783493649999997821, -44.99999999999997158, -95.57499999836127813 ) ) ;
#4873 = CARTESIAN_POINT ( 'NONE',  ( -37.06321265474346660, -32.25000000000000711, 7.063212654743582952 ) ) ;
#4874 = VERTEX_POINT ( 'NONE', #5870 ) ;
#4875 = ORIENTED_EDGE ( 'NONE', *, *, #7155, .T. ) ;
#4876 = CARTESIAN_POINT ( 'NONE',  ( -21.59636165304264921, -41.19859572486944188, 1.277368040863740228 ) ) ;
#4877 = CARTESIAN_POINT ( 'NONE',  ( -25.73429323749904185, -37.59859572486943335, -8.488613101951701267 ) ) ;
#4878 = CARTESIAN_POINT ( 'NONE',  ( -38.83610826798580717, -34.55140427513057233, 1.343104241417631073 ) ) ;
#4879 = ORIENTED_EDGE ( 'NONE', *, *, #7985, .F. ) ;
#4880 = CARTESIAN_POINT ( 'NONE',  ( 3.229347689422839895, -41.77065231057713390, -97.94999999890751496 ) ) ;
#4881 = CARTESIAN_POINT ( 'NONE',  ( -28.43739315969223824, -30.44999999999999574, -9.865911304835512041 ) ) ;
#4882 = FACE_OUTER_BOUND ( 'NONE', #2247, .T. ) ;
#4883 = CARTESIAN_POINT ( 'NONE',  ( 1.891708078845685481, -49.56698729999997255, -96.79999999890753770 ) ) ;
#4884 = CARTESIAN_POINT ( 'NONE',  ( -25.00000000000001776, -45.32948160161801354, 11.45643923738958847 ) ) ;
#4885 = CARTESIAN_POINT ( 'NONE',  ( -30.00000000000002487, 0.000000000000000000, -26.00000000000000355 ) ) ;
#4886 = ORIENTED_EDGE ( 'NONE', *, *, #1781, .T. ) ;
#4887 = CONICAL_SURFACE ( 'NONE', #8122, 1.649999999999998579, 1.029744258676653645 ) ;
#4888 = EDGE_CURVE ( 'NONE', #4891, #3552, #2444, .T. ) ;
#4889 = CARTESIAN_POINT ( 'NONE',  ( -36.28032828410546529, -33.24859572486943193, 6.359104887540839357 ) ) ;
#4890 = CARTESIAN_POINT ( 'NONE',  ( -31.56260684030781505, -31.95000000000000639, 9.865911304835510265 ) ) ;
#4891 = VERTEX_POINT ( 'NONE', #6444 ) ;
#4892 = CARTESIAN_POINT ( 'NONE',  ( -23.28248557872775137, -49.50000000000000711, 6.717514421272141156 ) ) ;
#4893 = DIRECTION ( 'NONE',  ( -0.000000000000000000, -0.000000000000000000, -1.000000000000000000 ) ) ;
#4894 = CARTESIAN_POINT ( 'NONE',  ( 4.566987299999998307, -43.10829192115428299, -99.79999999890752349 ) ) ;
#4895 = CARTESIAN_POINT ( 'NONE',  ( 4.999999999999998224, -44.99999999999997158, -100.0999999978150470 ) ) ;
#4896 = STYLED_ITEM ( 'NONE', ( #2267 ), #5903 ) ;
#4897 = CARTESIAN_POINT ( 'NONE',  ( -4.566987299999998307, -43.10829192115428299, -99.29999999890752349 ) ) ;
#4898 = CIRCLE ( 'NONE', #8684, 2.149999999999985256 ) ;
#4899 = CARTESIAN_POINT ( 'NONE',  ( -22.40239342223677355, -44.90140427513058086, -3.811716262761597473 ) ) ;
#4900 = VECTOR ( 'NONE', #5081, 1000.000000000000000 ) ;
#4901 = CARTESIAN_POINT ( 'NONE',  ( -2.071067811865475061, -39.99999999999997158, -95.95000000000003126 ) ) ;
#4902 = CARTESIAN_POINT ( 'NONE',  ( -3.229347689422839451, -48.22934768942280925, -96.74999999890752633 ) ) ;
#4903 = CARTESIAN_POINT ( 'NONE',  ( -31.39812190974910422, -40.95000000000000995, 8.827394325379140483 ) ) ;
#4904 = FACE_OUTER_BOUND ( 'NONE', #4206, .T. ) ;
#4905 = CARTESIAN_POINT ( 'NONE',  ( -26.14108075221394856, -39.60000000000000853, -7.573555455601170827 ) ) ;
#4906 =( BOUNDED_CURVE ( )  B_SPLINE_CURVE ( 2, ( #4750, #4046, #27, #2728, #3216, #5899, #640, #1180, #6592 ),
 .UNSPECIFIED., .F., .T. ) 
 B_SPLINE_CURVE_WITH_KNOTS ( ( 3, 2, 2, 2, 3 ),
 ( 0.2142857142857142738, 0.2321428571428571508, 0.2499999999999999722, 0.2678571428571427937, 0.2857142857142856429 ),
 .UNSPECIFIED. ) 
 CURVE ( )  GEOMETRIC_REPRESENTATION_ITEM ( )  RATIONAL_B_SPLINE_CURVE ( ( 1.000000000000000000, 0.9238795325112867385, 1.000000000000000000, 0.9238795325112867385, 1.000000000000000000, 0.9238795325112867385, 1.000000000000000000, 0.9238795325112869605, 0.9999999999999997780 ) ) 
 REPRESENTATION_ITEM ( '' )  );
#4907 = CARTESIAN_POINT ( 'NONE',  ( -30.00000000000000000, 0.000000000000000000, 80.00000000000002842 ) ) ;
#4908 = CARTESIAN_POINT ( 'NONE',  ( -30.00000000000002842, 0.000000000000000000, -25.00000000000000000 ) ) ;
#4909 = CARTESIAN_POINT ( 'NONE',  ( -23.28248557872775137, -31.50000000000000711, 6.717514421272141156 ) ) ;
#4910 = CARTESIAN_POINT ( 'NONE',  ( -41.99999999999996447, 22.00000000000000000, 60.00000000000002842 ) ) ;
#4911 = CARTESIAN_POINT ( 'NONE',  ( -38.90016716647221529, -35.85000000000000142, -4.534861676072185155 ) ) ;
#4912 = PRESENTATION_STYLE_ASSIGNMENT (( #4250 ) ) ;
#4913 = ORIENTED_EDGE ( 'NONE', *, *, #6300, .F. ) ;
#4914 = FACE_OUTER_BOUND ( 'NONE', #1389, .T. ) ;
#4915 = ORIENTED_EDGE ( 'NONE', *, *, #465, .T. ) ;
#4916 = CARTESIAN_POINT ( 'NONE',  ( -37.54950433343896776, -39.39859572486943762, 3.906122232810848249 ) ) ;
#4917 = CARTESIAN_POINT ( 'NONE',  ( -25.41550616830297571, -50.64859572486944472, 8.874878320068054549 ) ) ;
#4918 = CARTESIAN_POINT ( 'NONE',  ( -28.38237549136062654, -47.45140427513057091, -9.857197362228843573 ) ) ;
#4919 = ORIENTED_EDGE ( 'NONE', *, *, #4043, .F. ) ;
#4920 = CARTESIAN_POINT ( 'NONE',  ( -1.891708078845683039, -40.43301269999998482, -96.99999999890752633 ) ) ;
#4921 = CARTESIAN_POINT ( 'NONE',  ( -21.53543802021056663, -30.90000000000000924, -4.312909747525783821 ) ) ;
#4922 = FACE_OUTER_BOUND ( 'NONE', #8378, .T. ) ;
#4923 = CARTESIAN_POINT ( 'NONE',  ( -1.891708078845683483, -49.56698729999997255, -97.69999999890751496 ) ) ;
#4924 = DIRECTION ( 'NONE',  ( -0.000000000000000000, -0.000000000000000000, -1.000000000000000000 ) ) ;
#4925 = PLANE ( 'NONE',  #6278 ) ;
#4926 = EDGE_LOOP ( 'NONE', ( #6013, #4759, #673, #5538 ) ) ;
#4927 = CARTESIAN_POINT ( 'NONE',  ( -25.89286002894218086, -38.64859572486943762, 7.938018618334153231 ) ) ;
#4928 = CARTESIAN_POINT ( 'NONE',  ( -39.86591130483550671, -41.55000000000001137, 1.562606840307984468 ) ) ;
#4929 = ORIENTED_EDGE ( 'NONE', *, *, #130, .T. ) ;
#4930 = CARTESIAN_POINT ( 'NONE',  ( -39.38303923565386100, -50.70000000000000995, -1.486127417882099788 ) ) ;
#4931 = DIRECTION ( 'NONE',  ( -0.000000000000000000, -0.000000000000000000, -1.000000000000000000 ) ) ;
#4932 = FACE_OUTER_BOUND ( 'NONE', #3511, .T. ) ;
#4933 = CARTESIAN_POINT ( 'NONE',  ( -3.535533905932736864, -41.46446609406723383, -99.79999999781504982 ) ) ;
#4934 = CARTESIAN_POINT ( 'NONE',  ( -2.071067811865475505, -49.99999999999997158, -97.94999999781505551 ) ) ;
#4935 = CARTESIAN_POINT ( 'NONE',  ( -2.796473189345805913E-16, -40.43301269999997061, -99.44999999890752918 ) ) ;
#4936 = ADVANCED_FACE ( 'NONE', ( #6356 ), #3843, .T. ) ;
#4937 = EDGE_LOOP ( 'NONE', ( #2636, #7151, #2088, #1627 ) ) ;
#4938 = CARTESIAN_POINT ( 'NONE',  ( -36.31971658582311591, -32.25000000000000711, 6.319716585823199395 ) ) ;
#4939 = CIRCLE ( 'NONE', #5072, 12.49999999999998401 ) ;
#4940 = EDGE_CURVE ( 'NONE', #5958, #8507, #7730, .T. ) ;
#4941 = CIRCLE ( 'NONE', #560, 2.149999999999985256 ) ;
#4942 = CARTESIAN_POINT ( 'NONE',  ( 3.535533905932737309, -48.53553390593270933, -98.69300000002183992 ) ) ;
#4943 = DIRECTION ( 'NONE',  ( 1.000000000000000000, 0.000000000000000000, 0.000000000000000000 ) ) ;
#4944 = CARTESIAN_POINT ( 'NONE',  ( 4.999999999999998224, -44.99999999999997158, -96.09999999781504698 ) ) ;
#4945 = CARTESIAN_POINT ( 'NONE',  ( -25.64110105645932336, 9.000000000000001776, 124.0000000000000000 ) ) ;
#4946 = EDGE_CURVE ( 'NONE', #2486, #6859, #1026, .T. ) ;
#4947 = CARTESIAN_POINT ( 'NONE',  ( 2.000000000000000000, -1.773042676681341634, 2.493664996716660198E-15 ) ) ;
#4948 = CARTESIAN_POINT ( 'NONE',  ( -21.60464910494133406, -43.20000000000000995, 1.329692952841886155 ) ) ;
#4949 = EDGE_CURVE ( 'NONE', #3069, #2202, #3073, .T. ) ;
#4950 = CARTESIAN_POINT ( 'NONE',  ( 26.23795701647085821, -41.69067313909253869, 11.92283337402247767 ) ) ;
#4951 = CARTESIAN_POINT ( 'NONE',  ( -22.93678734525658314, -42.75000000000001421, -7.063212654743582952 ) ) ;
#4952 = LINE ( 'NONE', #7463, #3340 ) ;
#4953 = CARTESIAN_POINT ( 'NONE',  ( -20.13408869516453947, -34.04999999999998295, -1.562606840307983136 ) ) ;
#4954 = DIRECTION ( 'NONE',  ( 1.000000000000000000, 0.000000000000000000, 0.000000000000000000 ) ) ;
#4955 = CARTESIAN_POINT ( 'NONE',  ( -21.09983283352783801, -40.34999999999999432, 4.534861676072186043 ) ) ;
#4956 = VERTEX_POINT ( 'NONE', #1690 ) ;
#4957 = CYLINDRICAL_SURFACE ( 'NONE', #6556, 2.149999999999985256 ) ;
#4958 = VERTEX_POINT ( 'NONE', #4380 ) ;
#4959 = CARTESIAN_POINT ( 'NONE',  ( -38.81868038277247734, -42.54859572486944330, 1.453139578080855365 ) ) ;
#4960 = ADVANCED_FACE ( 'NONE', ( #5125 ), #7816, .T. ) ;
#4961 = CARTESIAN_POINT ( 'NONE',  ( -39.39132668755255651, -48.69859572486944188, -1.433802505903950308 ) ) ;
#4962 = CARTESIAN_POINT ( 'NONE',  ( -21.61293655684001536, -33.20140427513057091, 1.382017864820032971 ) ) ;
#4963 = CARTESIAN_POINT ( 'NONE',  ( -1.891708078845683039, -40.43301269999998482, -96.19999999890752918 ) ) ;
#4964 = CARTESIAN_POINT ( 'NONE',  ( -22.93678734525658314, -30.75000000000000000, -7.063212654743582952 ) ) ;
#4965 = AXIS2_PLACEMENT_3D ( 'NONE', #2342, #4532, #7884 ) ;
#4966 = LINE ( 'NONE', #7649, #8549 ) ;
#4967 = CARTESIAN_POINT ( 'NONE',  ( 4.566987299999998307, -43.10829192115428299, -96.59999999890753486 ) ) ;
#4968 = CARTESIAN_POINT ( 'NONE',  ( -29.66610994519569644, -49.99999999999997868, 12.49999999999998401 ) ) ;
#4969 = CARTESIAN_POINT ( 'NONE',  ( 4.566987300000000083, -46.89170807884565306, -98.29999999890752349 ) ) ;
#4970 = CARTESIAN_POINT ( 'NONE',  ( -26.64110105645932336, 10.00000000000000178, -25.00000000000000000 ) ) ;
#4971 = ORIENTED_EDGE ( 'NONE', *, *, #7586, .F. ) ;
#4972 = CARTESIAN_POINT ( 'NONE',  ( -21.59636165304264921, -44.19859572486944899, 1.277368040863740228 ) ) ;
#4973 = ADVANCED_FACE ( 'NONE', ( #4462 ), #7065, .F. ) ;
#4974 = CARTESIAN_POINT ( 'NONE',  ( -20.61696076434619584, -46.20000000000000284, 1.486127417882100676 ) ) ;
#4975 = VECTOR ( 'NONE', #659, 1000.000000000000000 ) ;
#4976 = EDGE_CURVE ( 'NONE', #120, #4648, #1109, .T. ) ;
#4977 = ORIENTED_EDGE ( 'NONE', *, *, #8448, .T. ) ;
#4978 = CARTESIAN_POINT ( 'NONE',  ( -21.51138689804841420, -29.90140427513058796, -4.265706762501151772 ) ) ;
#4979 = FACE_OUTER_BOUND ( 'NONE', #1677, .T. ) ;
#4980 = CARTESIAN_POINT ( 'NONE',  ( 3.535533905932736420, -41.46446609406723383, -98.39999999781504414 ) ) ;
#4981 = CARTESIAN_POINT ( 'NONE',  ( 5.000000000000000000, -47.07106781186545419, -99.34999999781506119 ) ) ;
#4982 = DIRECTION ( 'NONE',  ( -1.000000000000000000, 0.000000000000000000, 0.000000000000000000 ) ) ;
#4983 = CARTESIAN_POINT ( 'NONE',  ( 4.566987299999998307, -43.10829192115428299, -97.19999999890752918 ) ) ;
#4984 = VERTEX_POINT ( 'NONE', #2404 ) ;
#4985 = CARTESIAN_POINT ( 'NONE',  ( -36.01040764008574513, -30.00000000000000711, -6.010407640085605685 ) ) ;
#4986 = AXIS2_PLACEMENT_3D ( 'NONE', #1246, #671, #3988 ) ;
#4987 = CARTESIAN_POINT ( 'NONE',  ( 3.535533905932737309, -48.53553390593270933, -99.49300000002185129 ) ) ;
#4988 = DIRECTION ( 'NONE',  ( 0.000000000000000000, 0.000000000000000000, -1.000000000000000000 ) ) ;
#4989 = CARTESIAN_POINT ( 'NONE',  ( -38.39535089505872634, -50.70000000000000995, -1.329692952841885267 ) ) ;
#4990 = CARTESIAN_POINT ( 'NONE',  ( -18.00000000000023093, 1.469576158976798506E-15, -29.65000000000000213 ) ) ;
#4991 = AXIS2_PLACEMENT_3D ( 'NONE', #1321, #7010, #5689 ) ;
#4992 = CARTESIAN_POINT ( 'NONE',  ( -38.39535089505872634, -38.70000000000000284, -1.329692952841885267 ) ) ;
#4993 = B_SPLINE_CURVE_WITH_KNOTS ( 'NONE', 3,
 ( #1091, #417, #458, #3173, #8541, #7710, #1669, #8502, #2464, #5146, #2509, #4360, #6379, #3871, #6548, #500, #4528, #7214, #1176, #1190 ),
 .UNSPECIFIED., .F., .F.,
 ( 4, 2, 2, 2, 2, 2, 2, 2, 2, 4 ),
 ( 0.000000000000000000, 0.0009878455431463928783, 0.001975691086292775782, 0.002963536629439158469, 0.003951382172585541155, 0.004939227715731924276, 0.005927073258878306529, 0.006420996030451498089, 0.006914918802024691384, 0.007902764345171094454 ),
 .UNSPECIFIED. ) ;
#4994 = CARTESIAN_POINT ( 'NONE',  ( 3.229347689422841228, -48.22934768942280925, -95.94999999890751496 ) ) ;
#4995 = FACE_OUTER_BOUND ( 'NONE', #3296, .T. ) ;
#4996 = CARTESIAN_POINT ( 'NONE',  ( -28.51387258211773812, -31.80000000000000782, 9.383039235653802379 ) ) ;
#4997 = DIRECTION ( 'NONE',  ( -0.000000000000000000, -0.000000000000000000, 1.000000000000000000 ) ) ;
#4998 = CARTESIAN_POINT ( 'NONE',  ( -39.38303923565386100, -44.70000000000000284, -1.486127417882099788 ) ) ;
#4999 = VERTEX_POINT ( 'NONE', #4337 ) ;
#5000 = DIRECTION ( 'NONE',  ( -1.000000000000000000, -0.000000000000000000, -0.000000000000000000 ) ) ;
#5001 = ORIENTED_EDGE ( 'NONE', *, *, #1812, .F. ) ;
#5002 = CARTESIAN_POINT ( 'NONE',  ( -37.54950433343896776, -42.39859572486944472, 3.906122232810848249 ) ) ;
#5003 = CARTESIAN_POINT ( 'NONE',  ( -20.60867331244750034, -47.19859572486943478, 1.433802505903951419 ) ) ;
#5004 = CARTESIAN_POINT ( 'NONE',  ( -31.27736804086391942, -32.30140427513056522, -8.403638346957361449 ) ) ;
#5005 = ADVANCED_FACE ( 'NONE', ( #3720 ), #3801, .T. ) ;
#5006 = CARTESIAN_POINT ( 'NONE',  ( -4.566987299999998307, -44.99999999999997158, -100.0499999989075235 ) ) ;
#5007 = CARTESIAN_POINT ( 'NONE',  ( 31.62327852896863689, -40.25949688271492732, 12.39792973884353344 ) ) ;
#5008 = DIRECTION ( 'NONE',  ( 1.000000000000000000, 0.000000000000000000, 0.000000000000000000 ) ) ;
#5009 = PRODUCT_DEFINITION_SHAPE ( 'NONE', 'NONE',  #4320 ) ;
#5010 = CARTESIAN_POINT ( 'NONE',  ( -4.566987299999997418, -46.89170807884566727, -96.19999999890751496 ) ) ;
#5011 = CARTESIAN_POINT ( 'NONE',  ( -28.69222302389759705, -49.83705382567077891, 12.43557624291737795 ) ) ;
#5012 = AXIS2_PLACEMENT_3D ( 'NONE', #8307, #758, #2181 ) ;
#5013 = CARTESIAN_POINT ( 'NONE',  ( 1.891708078845682595, -40.43301269999998482, -97.29999999890750928 ) ) ;
#5014 = CARTESIAN_POINT ( 'NONE',  ( 0.000000000000000000, -1.773042676681341634, 2.493664996716660198E-15 ) ) ;
#5015 = EDGE_LOOP ( 'NONE', ( #2593, #8416, #5193, #4758 ) ) ;
#5016 = CARTESIAN_POINT ( 'NONE',  ( -34.10713997105786888, -40.14859572486943762, -7.938018618334151455 ) ) ;
#5017 = CARTESIAN_POINT ( 'NONE',  ( -28.43739315969223824, -45.45000000000000995, -9.865911304835512041 ) ) ;
#5018 = ORIENTED_EDGE ( 'NONE', *, *, #1574, .F. ) ;
#5019 = CARTESIAN_POINT ( 'NONE',  ( -28.56619749409589204, -30.80140427513057233, 9.391326687552490782 ) ) ;
#5020 = DIRECTION ( 'NONE',  ( -1.000000000000000000, 0.000000000000000000, 0.000000000000000000 ) ) ;
#5021 = CARTESIAN_POINT ( 'NONE',  ( -1.891708078845683039, -40.43301269999998482, -100.3999999989075178 ) ) ;
#5022 = CARTESIAN_POINT ( 'NONE',  ( 2.071067811865477282, -49.99999999999996447, -99.44999999781505551 ) ) ;
#5023 = DIRECTION ( 'NONE',  ( -0.000000000000000000, -0.000000000000000000, -1.000000000000000000 ) ) ;
#5024 = CARTESIAN_POINT ( 'NONE',  ( 5.000000000000000000, -47.07106781186545419, -97.85000000000002274 ) ) ;
#5025 = ORIENTED_EDGE ( 'NONE', *, *, #8591, .F. ) ;
#5026 = CIRCLE ( 'NONE', #7981, 1.000000000000000888 ) ;
#5027 = CARTESIAN_POINT ( 'NONE',  ( -23.98959235991431171, -31.50000000000000711, 6.010407640085604797 ) ) ;
#5028 = ORIENTED_EDGE ( 'NONE', *, *, #1418, .F. ) ;
#5029 = UNCERTAINTY_MEASURE_WITH_UNIT (LENGTH_MEASURE( 1.000000000000000082E-05 ), #3763, 'distance_accuracy_value', 'NONE');
#5030 = PLANE ( 'NONE',  #2773 ) ;
#5031 = CARTESIAN_POINT ( 'NONE',  ( 3.535533905932737309, -48.53553390593270933, -96.19999999781504130 ) ) ;
#5032 = DIRECTION ( 'NONE',  ( 0.000000000000000000, 0.000000000000000000, -1.000000000000000000 ) ) ;
#5033 = CARTESIAN_POINT ( 'NONE',  ( -4.999999999999998224, -44.99999999999997158, -98.89999999781504414 ) ) ;
#5034 = VECTOR ( 'NONE', #979, 1000.000000000000000 ) ;
#5035 = CARTESIAN_POINT ( 'NONE',  ( -28.60187809025093841, -36.45000000000000284, -8.827394325379140483 ) ) ;
#5036 = DIRECTION ( 'NONE',  ( 0.000000000000000000, 0.000000000000000000, 1.000000000000000000 ) ) ;
#5037 = CARTESIAN_POINT ( 'NONE',  ( 2.071067811865474173, -39.99999999999997158, -98.45000000000000284 ) ) ;
#5038 = CARTESIAN_POINT ( 'NONE',  ( -21.09983283352784156, -31.34999999999999787, 4.534861676072186043 ) ) ;
#5039 = DIRECTION ( 'NONE',  ( -1.000000000000000000, 0.000000000000000000, 0.000000000000000000 ) ) ;
#5040 = CARTESIAN_POINT ( 'NONE',  ( -38.46456197978948666, -41.40000000000000568, 4.312909747525784709 ) ) ;
#5041 = FILL_AREA_STYLE_COLOUR ( '', #3405 ) ;
#5042 = VERTEX_POINT ( 'NONE', #8518 ) ;
#5043 = ORIENTED_EDGE ( 'NONE', *, *, #7792, .T. ) ;
#5044 = CARTESIAN_POINT ( 'NONE',  ( -36.28032828410546529, -39.24859572486943904, 6.359104887540839357 ) ) ;
#5045 = CARTESIAN_POINT ( 'NONE',  ( -23.24502507771338600, -44.49859572486944614, 6.680053920257780220 ) ) ;
#5046 = CARTESIAN_POINT ( 'NONE',  ( -36.35910488754074521, -34.25140427513057517, 6.280328284105565650 ) ) ;
#5047 = EDGE_CURVE ( 'NONE', #2177, #598, #2484, .T. ) ;
#5048 = LINE ( 'NONE', #327, #7269 ) ;
#5049 = CARTESIAN_POINT ( 'NONE',  ( 29.99999999999997158, 1.102182119232617753E-14, 80.00000000000002842 ) ) ;
#5050 = CARTESIAN_POINT ( 'NONE',  ( -28.51387258211773812, -40.80000000000000426, 9.383039235653802379 ) ) ;
#5051 = DIRECTION ( 'NONE',  ( -1.000000000000000000, 0.000000000000000000, 0.000000000000000000 ) ) ;
#5052 = CARTESIAN_POINT ( 'NONE',  ( -27.48298108591646738, -49.33233869400795868, 12.24706002614421507 ) ) ;
#5053 = CARTESIAN_POINT ( 'NONE',  ( 3.229347689422841228, -48.22934768942280925, -97.54999999890752349 ) ) ;
#5054 = FILL_AREA_STYLE_COLOUR ( '', #3821 ) ;
#5055 = ORIENTED_EDGE ( 'NONE', *, *, #2548, .T. ) ;
#5056 = CARTESIAN_POINT ( 'NONE',  ( -36.04786814110010340, -39.99859572486943904, -5.972947139071243861 ) ) ;
#5057 = CARTESIAN_POINT ( 'NONE',  ( -38.90016716647221529, -47.85000000000000853, -4.534861676072185155 ) ) ;
#5058 = ORIENTED_EDGE ( 'NONE', *, *, #6484, .T. ) ;
#5059 = CARTESIAN_POINT ( 'NONE',  ( -31.61762450863942320, -39.95140427513058512, 9.857197362228843573 ) ) ;
#5060 = CARTESIAN_POINT ( 'NONE',  ( -4.999999999999998224, -44.99999999999997158, -96.49999999781503845 ) ) ;
#5061 = DIRECTION ( 'NONE',  ( -1.000000000000000000, -0.000000000000000000, -0.000000000000000000 ) ) ;
#5062 = ADVANCED_FACE ( 'NONE', ( #1991 ), #4680, .T. ) ;
#5063 = CARTESIAN_POINT ( 'NONE',  ( -2.071067811865475061, -39.99999999999997158, -97.44999999781504130 ) ) ;
#5064 = DIRECTION ( 'NONE',  ( 1.000000000000000000, 0.000000000000000000, 0.000000000000000000 ) ) ;
#5065 = CARTESIAN_POINT ( 'NONE',  ( 9.184850993605145972E-16, -49.99999999999997158, -97.19999999999998863 ) ) ;
#5066 = B_SPLINE_CURVE_WITH_KNOTS ( 'NONE', 1,
 ( #8151, #3388 ),
 .UNSPECIFIED., .F., .F.,
 ( 2, 2 ),
 ( 0.000000000000000000, 1.000000000000000000 ),
 .UNSPECIFIED. ) ;
#5067 = ORIENTED_EDGE ( 'NONE', *, *, #5608, .T. ) ;
#5068 = CARTESIAN_POINT ( 'NONE',  ( -37.96330746473829976, -32.85000000000000853, -4.057507815433013754 ) ) ;
#5069 = ORIENTED_EDGE ( 'NONE', *, *, #3009, .T. ) ;
#5070 = CARTESIAN_POINT ( 'NONE',  ( 3.535533905932737309, -48.53553390593270933, -97.90000000000000568 ) ) ;
#5071 = CARTESIAN_POINT ( 'NONE',  ( -4.999999999999998224, -44.99999999999997158, -95.69999999781504130 ) ) ;
#5072 = AXIS2_PLACEMENT_3D ( 'NONE', #8268, #2319, #1069 ) ;
#5073 = DIRECTION ( 'NONE',  ( -0.000000000000000000, -0.000000000000000000, -1.000000000000000000 ) ) ;
#5074 = PLANE ( 'NONE',  #8062 ) ;
#5075 = CARTESIAN_POINT ( 'NONE',  ( -38.39535089505872634, -44.70000000000000284, -1.329692952841885267 ) ) ;
#5076 = PRODUCT_DEFINITION_SHAPE ( 'NONE', 'NONE',  #6796 ) ;
#5077 = CARTESIAN_POINT ( 'NONE',  ( -2.071067811865475061, -39.99999999999997158, -99.84999999781504698 ) ) ;
#5078 = FACE_OUTER_BOUND ( 'NONE', #3171, .T. ) ;
#5079 = CARTESIAN_POINT ( 'NONE',  ( -28.60187809025093841, -30.44999999999999574, -8.827394325379140483 ) ) ;
#5080 = CARTESIAN_POINT ( 'NONE',  ( -20.13408869516453947, -37.05000000000001137, -1.562606840307983136 ) ) ;
#5081 = DIRECTION ( 'NONE',  ( -0.000000000000000000, 1.000000000000000000, -0.000000000000000000 ) ) ;
#5082 = AXIS2_PLACEMENT_3D ( 'NONE', #3861, #5714, #6456 ) ;
#5083 = CARTESIAN_POINT ( 'NONE',  ( -31.48612741788231517, -39.30000000000001137, -9.383039235653804155 ) ) ;
#5084 =( NAMED_UNIT ( * ) SI_UNIT ( $, .STERADIAN. ) SOLID_ANGLE_UNIT ( ) );
#5085 = EDGE_LOOP ( 'NONE', ( #497, #810, #2115 ) ) ;
#5086 = CARTESIAN_POINT ( 'NONE',  ( -23.71967171589458445, -46.74859572486943904, -6.359104887540838469 ) ) ;
#5087 = CARTESIAN_POINT ( 'NONE',  ( -20.61696076434619584, -37.20000000000000284, 1.486127417882100676 ) ) ;
#5088 = CARTESIAN_POINT ( 'NONE',  ( -28.54686042191934092, -38.45140427513057801, -8.818680382772479120 ) ) ;
#5089 = STYLED_ITEM ( 'NONE', ( #716 ), #7491 ) ;
#5090 = CARTESIAN_POINT ( 'NONE',  ( 50.00000000000002842, -44.99999999999997158, 2.099999999999997868 ) ) ;
#5091 = DIRECTION ( 'NONE',  ( 0.000000000000000000, -0.000000000000000000, 1.000000000000000000 ) ) ;
#5092 = CARTESIAN_POINT ( 'NONE',  ( -38.46456197978948666, -41.40000000000000568, 4.312909747525784709 ) ) ;
#5093 = CARTESIAN_POINT ( 'NONE',  ( -4.566987299999998307, -43.10829192115428299, -99.49999999890754054 ) ) ;
#5094 = CYLINDRICAL_SURFACE ( 'NONE', #1317, 2.099999999999997868 ) ;
#5095 = CARTESIAN_POINT ( 'NONE',  ( -1.891708078845683039, -40.43301269999998482, -96.39999999890753202 ) ) ;
#5096 = ORIENTED_EDGE ( 'NONE', *, *, #515, .T. ) ;
#5097 = DIRECTION ( 'NONE',  ( -0.000000000000000000, -0.000000000000000000, -1.000000000000000000 ) ) ;
#5098 = AXIS2_PLACEMENT_3D ( 'NONE', #5998, #6611, #3279 ) ;
#5099 = EDGE_CURVE ( 'NONE', #864, #2721, #7232, .T. ) ;
#5100 = CARTESIAN_POINT ( 'NONE',  ( -37.98859631114233792, -45.84859572486944046, -4.007875659808334490 ) ) ;
#5101 = CARTESIAN_POINT ( 'NONE',  ( -20.13408869516453947, -49.04999999999999716, -1.562606840307983136 ) ) ;
#5102 = ORIENTED_EDGE ( 'NONE', *, *, #7524, .T. ) ;
#5103 = VECTOR ( 'NONE', #1816, 1000.000000000000000 ) ;
#5104 = CARTESIAN_POINT ( 'NONE',  ( -28.38237549136062654, -38.45140427513057801, -9.857197362228843573 ) ) ;
#5105 = CARTESIAN_POINT ( 'NONE',  ( 0.000000000000000000, -44.99999999999997158, -95.00000000000000000 ) ) ;
#5106 = DIRECTION ( 'NONE',  ( 1.000000000000000000, -0.000000000000000000, 0.000000000000000000 ) ) ;
#5107 = LINE ( 'NONE', #2550, #3273 ) ;
#5108 = CARTESIAN_POINT ( 'NONE',  ( 9.184850993605145972E-16, -49.99999999999997158, -96.40000000000000568 ) ) ;
#5109 = VERTEX_POINT ( 'NONE', #7366 ) ;
#5110 = CARTESIAN_POINT ( 'NONE',  ( -37.93801861833426159, -49.85140427513058370, -4.107139971057695682 ) ) ;
#5111 = AXIS2_PLACEMENT_3D ( 'NONE', #6383, #382, #5064 ) ;
#5112 = VECTOR ( 'NONE', #4574, 1000.000000000000000 ) ;
#5113 = ORIENTED_EDGE ( 'NONE', *, *, #786, .F. ) ;
#5114 = EDGE_CURVE ( 'NONE', #6251, #4620, #8243, .T. ) ;
#5115 = CARTESIAN_POINT ( 'NONE',  ( 3.535533905932736420, -41.46446609406723383, -96.90000000000000568 ) ) ;
#5116 = PRESENTATION_LAYER_ASSIGNMENT (  '', '', ( #3846 ) ) ;
#5117 = DIRECTION ( 'NONE',  ( 0.000000000000000000, 0.000000000000000000, -1.000000000000000000 ) ) ;
#5118 = CARTESIAN_POINT ( 'NONE',  ( -4.270064113631143243, -47.61730482574012058, -99.99930497888919945 ) ) ;
#5119 = CONTEXT_DEPENDENT_SHAPE_REPRESENTATION ( #633, #5684 ) ;
#5120 = FACE_OUTER_BOUND ( 'NONE', #2146, .T. ) ;
#5121 = CARTESIAN_POINT ( 'NONE',  ( -3.535533905932735532, -48.53553390593270933, -97.19999999781504130 ) ) ;
#5122 = DIRECTION ( 'NONE',  ( -0.000000000000000000, 1.000000000000000000, -0.000000000000000000 ) ) ;
#5123 = CARTESIAN_POINT ( 'NONE',  ( 0.1999999999999987899, 0.000000000000000000, 0.000000000000000000 ) ) ;
#5124 = VECTOR ( 'NONE', #5797, 1000.000000000000000 ) ;
#5125 = FACE_OUTER_BOUND ( 'NONE', #8278, .T. ) ;
#5126 = CARTESIAN_POINT ( 'NONE',  ( -25.68709025247441602, -39.60000000000000853, -8.464561979789547053 ) ) ;
#5127 = SHAPE_REPRESENTATION_RELATIONSHIP ( 'NONE' , 'NONE' ,  #7097, #4644 ) ;
#5128 = ORIENTED_EDGE ( 'NONE', *, *, #3277, .F. ) ;
#5129 = CARTESIAN_POINT ( 'NONE',  ( -31.38201786482021305, -49.29859572486945041, -8.387063443159975762 ) ) ;
#5130 = CARTESIAN_POINT ( 'NONE',  ( -39.86591130483550671, -35.55000000000001137, 1.562606840307984468 ) ) ;
#5131 = CARTESIAN_POINT ( 'NONE',  ( -21.61293655684001536, -39.20140427513058512, 1.382017864820032971 ) ) ;
#5132 = CARTESIAN_POINT ( 'NONE',  ( 3.229347689422841228, -48.22934768942280925, -98.94999999890752918 ) ) ;
#5133 = CARTESIAN_POINT ( 'NONE',  ( -33.35889894354067309, -7.999999999999996447, 124.0000000000000000 ) ) ;
#5134 = CARTESIAN_POINT ( 'NONE',  ( -23.28248557872775137, -37.50000000000000711, 6.717514421272141156 ) ) ;
#5135 = CARTESIAN_POINT ( 'NONE',  ( 19.99999999999997513, 1.224646799147352901E-14, 80.00000000000002842 ) ) ;
#5136 = CARTESIAN_POINT ( 'NONE',  ( -34.99999999999997868, -45.00000000000000000, 11.45643923738958847 ) ) ;
#5137 = CARTESIAN_POINT ( 'NONE',  ( 4.566987299999998307, -44.99999999999997158, -96.64999999890753202 ) ) ;
#5138 = FILL_AREA_STYLE ('',( #5054 ) ) ;
#5139 = ORIENTED_EDGE ( 'NONE', *, *, #2920, .T. ) ;
#5140 = PLANE ( 'NONE',  #4414 ) ;
#5141 = CARTESIAN_POINT ( 'NONE',  ( -23.71967171589458445, -49.74859572486944614, -6.359104887540838469 ) ) ;
#5142 = CARTESIAN_POINT ( 'NONE',  ( -38.87487832006816291, -31.85140427513056594, -4.584493831696867971 ) ) ;
#5143 = VERTEX_POINT ( 'NONE', #1011 ) ;
#5144 = CARTESIAN_POINT ( 'NONE',  ( -25.63988726744978663, -32.60140427513057659, -8.440510857627391061 ) ) ;
#5145 = AXIS2_PLACEMENT_3D ( 'NONE', #340, #6257, #3047 ) ;
#5146 = CARTESIAN_POINT ( 'NONE',  ( -33.76680408720224591, -48.30383393989879437, 11.92131216183668663 ) ) ;
#5147 = DIRECTION ( 'NONE',  ( -1.000000000000000000, 0.000000000000000000, 0.000000000000000000 ) ) ;
#5148 = CARTESIAN_POINT ( 'NONE',  ( -5.000000000000002665, -47.07106781186544708, -97.34999999999999432 ) ) ;
#5149 = ADVANCED_FACE ( 'NONE', ( #4725 ), #7277, .T. ) ;
#5150 = DIRECTION ( 'NONE',  ( 0.000000000000000000, 0.000000000000000000, 1.000000000000000000 ) ) ;
#5151 = CARTESIAN_POINT ( 'NONE',  ( 3.535533905932737309, -48.53553390593270933, -95.50000000000000000 ) ) ;
#5152 = VERTEX_POINT ( 'NONE', #8562 ) ;
#5153 =( REPRESENTATION_RELATIONSHIP ('NONE','NONE', #2265, #3450 ) REPRESENTATION_RELATIONSHIP_WITH_TRANSFORMATION ( #3015 )SHAPE_REPRESENTATION_RELATIONSHIP( ) );
#5154 = CARTESIAN_POINT ( 'NONE',  ( -33.85891924778610473, -47.10000000000000142, 7.573555455601171715 ) ) ;
#5155 = ORIENTED_EDGE ( 'NONE', *, *, #2286, .T. ) ;
#5156 = CARTESIAN_POINT ( 'NONE',  ( 9.184850993605145972E-16, -49.99999999999997158, -97.19999999999998863 ) ) ;
#5157 = CARTESIAN_POINT ( 'NONE',  ( 0.04104470510518735960, -50.00775265013817972, -99.99997323207621491 ) ) ;
#5158 = CARTESIAN_POINT ( 'NONE',  ( 0.1999999999999987899, 0.000000000000000000, 0.000000000000000000 ) ) ;
#5159 = DIRECTION ( 'NONE',  ( -0.000000000000000000, 1.000000000000000000, -0.000000000000000000 ) ) ;
#5160 = CARTESIAN_POINT ( 'NONE',  ( -4.999999999999998224, -46.91341716182541433, -94.94680602339629161 ) ) ;
#5161 = DIRECTION ( 'NONE',  ( -0.000000000000000000, 1.000000000000000000, -0.000000000000000000 ) ) ;
#5163 = EDGE_CURVE ( 'NONE', #5681, #580, #6018, .T. ) ;
#5162 = AXIS2_PLACEMENT_3D ( 'NONE', #6159, #2197, #1522 ) ;
#5164 = CARTESIAN_POINT ( 'NONE',  ( -25.64110105645932336, 9.000000000000001776, -24.00000000000000000 ) ) ;
#5165 = CARTESIAN_POINT ( 'NONE',  ( -33.35889894354067309, -7.999999999999996447, 125.0000000000000000 ) ) ;
#5166 = AXIS2_PLACEMENT_3D ( 'NONE', #7199, #6492, #366 ) ;
#5167 = ORIENTED_EDGE ( 'NONE', *, *, #3375, .F. ) ;
#5168 = CARTESIAN_POINT ( 'NONE',  ( -21.18131961722757595, -47.04859572486944330, -1.453139578080854699 ) ) ;
#5169 = AXIS2_PLACEMENT_3D ( 'NONE', #5543, #125, #739 ) ;
#5170 = CARTESIAN_POINT ( 'NONE',  ( -34.31290974752564438, -32.10000000000000142, 8.464561979789547053 ) ) ;
#5171 = CARTESIAN_POINT ( 'NONE',  ( -23.64089511245930098, -38.75140427513058228, -6.280328284105564762 ) ) ;
#5172 = CARTESIAN_POINT ( 'NONE',  ( -1.891708078845683705, -49.56698729999997255, -99.89999999890753202 ) ) ;
#5173 = CARTESIAN_POINT ( 'NONE',  ( 34.32699982994827081, -42.48926715326577863, 11.72748501658993625 ) ) ;
#5174 = CARTESIAN_POINT ( 'NONE',  ( -36.75497492228666374, -39.99859572486943904, -6.680053920257780220 ) ) ;
#5175 = CARTESIAN_POINT ( 'NONE',  ( -28.51387258211773812, -34.80000000000000426, 9.383039235653802379 ) ) ;
#5176 = CARTESIAN_POINT ( 'NONE',  ( -36.01040764008574513, -30.00000000000000711, -6.010407640085605685 ) ) ;
#5177 = CARTESIAN_POINT ( 'NONE',  ( -44.14999999999995595, 22.00000000000000000, 80.00000000000002842 ) ) ;
#5178 = CARTESIAN_POINT ( 'NONE',  ( 1.891708078845685481, -49.56698729999997255, -95.79999999890752349 ) ) ;
#5179 = ORIENTED_EDGE ( 'NONE', *, *, #1988, .T. ) ;
#5180 = CARTESIAN_POINT ( 'NONE',  ( -33.35889894354067309, 9.000000000000001776, -24.00000000000000000 ) ) ;
#5181 = CARTESIAN_POINT ( 'NONE',  ( -38.40363834695740053, -48.69859572486944188, -1.277368040863739118 ) ) ;
#5182 = CARTESIAN_POINT ( 'NONE',  ( -21.09983283352784156, -49.35000000000000853, 4.534861676072186043 ) ) ;
#5183 = VERTEX_POINT ( 'NONE', #2037 ) ;
#5184 = VERTEX_POINT ( 'NONE', #563 ) ;
#5185 = CARTESIAN_POINT ( 'NONE',  ( -31.43380250590416125, -35.30140427513057944, -9.391326687552492558 ) ) ;
#5186 = DIRECTION ( 'NONE',  ( -0.000000000000000000, -0.000000000000000000, -1.000000000000000000 ) ) ;
#5187 = CARTESIAN_POINT ( 'NONE',  ( -30.00000000000000000, -49.99999999999997158, -12.49999999999997335 ) ) ;
#5188 = CARTESIAN_POINT ( 'NONE',  ( -41.99999999999996447, 48.00000000000002842, -22.00000000000000000 ) ) ;
#5189 = CARTESIAN_POINT ( 'NONE',  ( -3.535533905932736864, -41.46446609406723383, -96.70000000000000284 ) ) ;
#5190 = ORIENTED_EDGE ( 'NONE', *, *, #2254, .F. ) ;
#5191 = CARTESIAN_POINT ( 'NONE',  ( -37.57355545560112375, -38.40000000000000568, 3.858919247786223305 ) ) ;
#5192 = EDGE_CURVE ( 'NONE', #3431, #3121, #3276, .T. ) ;
#5193 = ORIENTED_EDGE ( 'NONE', *, *, #4542, .T. ) ;
#5194 = CARTESIAN_POINT ( 'NONE',  ( 4.999999999999998224, -44.99999999999997158, -97.00000000000000000 ) ) ;
#5195 = CARTESIAN_POINT ( 'NONE',  ( 3.930156119229561540, -41.85908832164993498, -99.99888990999863836 ) ) ;
#5196 = CARTESIAN_POINT ( 'NONE',  ( -21.61293655684001536, -36.20140427513057091, 1.382017864820032971 ) ) ;
#5197 = EDGE_CURVE ( 'NONE', #1925, #6933, #3770, .T. ) ;
#5198 = CARTESIAN_POINT ( 'NONE',  ( -2.071067811865475505, -49.99999999999997158, -97.14999999781504414 ) ) ;
#5199 = AXIS2_PLACEMENT_3D ( 'NONE', #7855, #5161, #1820 ) ;
#5200 = CARTESIAN_POINT ( 'NONE',  ( -31.32969295284206979, -36.30000000000000426, -8.395350895058669494 ) ) ;
#5201 = CARTESIAN_POINT ( 'NONE',  ( -30.00000000000000000, -45.00000000000000000, 30.00000000000000000 ) ) ;
#5202 = EDGE_CURVE ( 'NONE', #3178, #4594, #2702, .T. ) ;
#5203 = CARTESIAN_POINT ( 'NONE',  ( -39.38303923565386100, -47.70000000000000284, -1.486127417882099788 ) ) ;
#5204 = DIRECTION ( 'NONE',  ( 6.123233995736766036E-17, -1.000000000000000000, 0.000000000000000000 ) ) ;
#5205 = VERTEX_POINT ( 'NONE', #3975 ) ;
#5206 = CARTESIAN_POINT ( 'NONE',  ( -26.18828373723858149, -49.59859572486944046, -7.597606577763319713 ) ) ;
#5207 = CARTESIAN_POINT ( 'NONE',  ( -31.48612741788231517, -36.30000000000000426, -9.383039235653804155 ) ) ;
#5208 = CARTESIAN_POINT ( 'NONE',  ( -28.54686042191934092, -35.45140427513057801, -8.818680382772479120 ) ) ;
#5209 = ADVANCED_FACE ( 'NONE', ( #8648 ), #8135, .T. ) ;
#5210 = DIRECTION ( 'NONE',  ( 0.000000000000000000, 0.000000000000000000, -1.000000000000000000 ) ) ;
#5211 =( GEOMETRIC_REPRESENTATION_CONTEXT ( 3 ) GLOBAL_UNCERTAINTY_ASSIGNED_CONTEXT ( ( #4859 ) ) GLOBAL_UNIT_ASSIGNED_CONTEXT ( ( #372, #7703, #8415 ) ) REPRESENTATION_CONTEXT ( 'NONE', 'WORKASPACE' ) );
#5212 = DIRECTION ( 'NONE',  ( 0.000000000000000000, 0.000000000000000000, 1.000000000000000000 ) ) ;
#5213 = CARTESIAN_POINT ( 'NONE',  ( -25.41550616830297571, -41.64859572486943762, 8.874878320068054549 ) ) ;
#5214 = CARTESIAN_POINT ( 'NONE',  ( -22.93678734525658314, -39.74999999999999289, -7.063212654743582952 ) ) ;
#5215 = CARTESIAN_POINT ( 'NONE',  ( -4.566987299999997418, -46.89170807884566727, -100.1999999989075150 ) ) ;
#5216 = CARTESIAN_POINT ( 'NONE',  ( 42.00000000000000711, 60.00000000000002842, -23.64999999999992042 ) ) ;
#5217 = CARTESIAN_POINT ( 'NONE',  ( -3.229347689422840784, -41.77065231057713390, -100.3499999989075206 ) ) ;
#5218 = ORIENTED_EDGE ( 'NONE', *, *, #3138, .F. ) ;
#5219 = DIRECTION ( 'NONE',  ( -0.000000000000000000, -0.000000000000000000, -1.000000000000000000 ) ) ;
#5220 = CARTESIAN_POINT ( 'NONE',  ( -25.89286002894218086, -50.64859572486944472, 7.938018618334153231 ) ) ;
#5221 = CARTESIAN_POINT ( 'NONE',  ( -34.48522952044771017, -35.15140427513058086, -8.925456012876139766 ) ) ;
#5222 = ORIENTED_EDGE ( 'NONE', *, *, #3659, .F. ) ;
#5223 = CARTESIAN_POINT ( 'NONE',  ( -28.56619749409589204, -33.80140427513056522, 9.391326687552490782 ) ) ;
#5224 = CARTESIAN_POINT ( 'NONE',  ( -41.99999999999996447, 60.00000000000002842, 22.00000000000000000 ) ) ;
#5225 = CARTESIAN_POINT ( 'NONE',  ( -4.999999999999998224, -42.92893218813449607, -99.04999999999999716 ) ) ;
#5226 = CARTESIAN_POINT ( 'NONE',  ( -4.999999999999997335, -47.07106781186546129, -96.44999999781505551 ) ) ;
#5227 = FACE_OUTER_BOUND ( 'NONE', #7877, .T. ) ;
#5228 = PLANE ( 'NONE',  #4312 ) ;
#5229 = EDGE_CURVE ( 'NONE', #2721, #2177, #2791, .T. ) ;
#5230 = ORIENTED_EDGE ( 'NONE', *, *, #5192, .T. ) ;
#5231 = CARTESIAN_POINT ( 'NONE',  ( -38.82739432537914581, -38.54999999999999716, 1.398121909749243441 ) ) ;
#5232 = AXIS2_PLACEMENT_3D ( 'NONE', #341, #1003, #7044 ) ;
#5233 = EDGE_CURVE ( 'NONE', #3140, #58, #101, .T. ) ;
#5234 = ORIENTED_EDGE ( 'NONE', *, *, #6999, .T. ) ;
#5235 = CARTESIAN_POINT ( 'NONE',  ( -30.00000000000002487, 0.000000000000000000, -29.65000000000000213 ) ) ;
#5236 = CARTESIAN_POINT ( 'NONE',  ( -4.999999999999998224, -44.99999999999997158, -96.60000000000000853 ) ) ;
#5237 = CARTESIAN_POINT ( 'NONE',  ( -20.61696076434619584, -43.20000000000000995, 1.486127417882100676 ) ) ;
#5238 = CARTESIAN_POINT ( 'NONE',  ( -1.891708078845683483, -49.56698729999997255, -97.49999999890754054 ) ) ;
#5239 = AXIS2_PLACEMENT_3D ( 'NONE', #7799, #7925, #6635 ) ;
#5240 = CARTESIAN_POINT ( 'NONE',  ( 4.472107766621025604, -47.30873943526144387, -100.0006001545488203 ) ) ;
#5241 = CARTESIAN_POINT ( 'NONE',  ( -33.90612223281073057, -34.10140427513057659, 7.549504333439023718 ) ) ;
#5242 = DIRECTION ( 'NONE',  ( -1.000000000000000000, -0.000000000000000000, -0.000000000000000000 ) ) ;
#5243 = CARTESIAN_POINT ( 'NONE',  ( -31.39812190974910422, -31.95000000000000639, 8.827394325379140483 ) ) ;
#5244 = CARTESIAN_POINT ( 'NONE',  ( -2.071067811865475061, -39.99999999999997158, -97.54999999999998295 ) ) ;
#5245 = DIRECTION ( 'NONE',  ( 0.000000000000000000, 0.000000000000000000, 1.000000000000000000 ) ) ;
#5246 = DIRECTION ( 'NONE',  ( 0.000000000000000000, 0.000000000000000000, 1.000000000000000000 ) ) ;
#5247 = ORIENTED_EDGE ( 'NONE', *, *, #5099, .T. ) ;
#5248 = CARTESIAN_POINT ( 'NONE',  ( -28.61798213517984024, -50.79859572486945041, 8.387063443159973986 ) ) ;
#5249 = CARTESIAN_POINT ( 'NONE',  ( -37.06321265474346660, -38.25000000000001421, 7.063212654743582952 ) ) ;
#5250 = CARTESIAN_POINT ( 'NONE',  ( -21.16389173201424612, -42.05140427513057944, -1.343104241417630185 ) ) ;
#5251 = FACE_BOUND ( 'NONE', #2014, .T. ) ;
#5252 = FACE_OUTER_BOUND ( 'NONE', #6468, .T. ) ;
#5253 = CARTESIAN_POINT ( 'NONE',  ( -20.60867331244750034, -38.19859572486942767, 1.433802505903951419 ) ) ;
#5254 = CARTESIAN_POINT ( 'NONE',  ( -31.48612741788231517, -42.30000000000000426, -9.383039235653804155 ) ) ;
#5255 = CARTESIAN_POINT ( 'NONE',  ( -50.00000000000002842, 30.00000000000000000, 80.00000000000002842 ) ) ;
#5256 = CARTESIAN_POINT ( 'NONE',  ( -25.64110105645932336, -8.999999999999998224, -24.00000000000000000 ) ) ;
#5257 = CARTESIAN_POINT ( 'NONE',  ( -4.566987299999998307, -43.10829192115428299, -100.2999999989075093 ) ) ;
#5258 = ORIENTED_EDGE ( 'NONE', *, *, #1937, .F. ) ;
#5259 = CARTESIAN_POINT ( 'NONE',  ( 2.000000000000000000, -1.329782007511006725, -0.7677499999999984892 ) ) ;
#5260 = CARTESIAN_POINT ( 'NONE',  ( -28.65689575858256077, -49.44859572486943478, -8.836108267985801845 ) ) ;
#5261 = CARTESIAN_POINT ( 'NONE',  ( -21.51138689804841420, -35.90140427513058086, -4.265706762501151772 ) ) ;
#5262 = ORIENTED_EDGE ( 'NONE', *, *, #3105, .T. ) ;
#5263 = EDGE_LOOP ( 'NONE', ( #2384, #2588, #8109, #3595 ) ) ;
#5264 = CARTESIAN_POINT ( 'NONE',  ( -38.48861310195163554, -46.40140427513058086, 4.265706762501153548 ) ) ;
#5265 = DIRECTION ( 'NONE',  ( 0.000000000000000000, 0.000000000000000000, 1.000000000000000000 ) ) ;
#5266 = DIRECTION ( 'NONE',  ( 0.000000000000000000, 0.000000000000000000, -1.000000000000000000 ) ) ;
#5267 = CARTESIAN_POINT ( 'NONE',  ( -3.061616997868382155E-16, -39.99999999999997158, -98.29999999781504982 ) ) ;
#5268 = CARTESIAN_POINT ( 'NONE',  ( -20.00000000000002487, 0.000000000000000000, -45.00000000000000000 ) ) ;
#5269 = CARTESIAN_POINT ( 'NONE',  ( 3.535533905932737309, -48.53553390593270933, -99.50000000000000000 ) ) ;
#5270 = ORIENTED_EDGE ( 'NONE', *, *, #8199, .T. ) ;
#5271 = CARTESIAN_POINT ( 'NONE',  ( -34.05750781543318340, -42.15000000000001279, -7.963307464738195840 ) ) ;
#5272 = DIRECTION ( 'NONE',  ( -0.000000000000000000, -0.000000000000000000, 1.000000000000000000 ) ) ;
#5273 = CARTESIAN_POINT ( 'NONE',  ( 0.1999999999999987899, 0.000000000000000000, 0.000000000000000000 ) ) ;
#5274 = CARTESIAN_POINT ( 'NONE',  ( -3.061616997868382155E-16, -39.99999999999997158, -95.89999999781505835 ) ) ;
#5275 = CARTESIAN_POINT ( 'NONE',  ( -25.46513832392765408, -43.64999999999999147, 8.900167166472096270 ) ) ;
#5276 = CARTESIAN_POINT ( 'NONE',  ( -4.566987299999997418, -46.89170807884566727, -98.39999999890753202 ) ) ;
#5277 = CARTESIAN_POINT ( 'NONE',  ( 1.168677208981296678, -49.87010530342148940, -100.0006950213451233 ) ) ;
#5278 = CARTESIAN_POINT ( 'NONE',  ( -31.45313957808072303, -30.95140427513058157, 8.818680382772479120 ) ) ;
#5279 = CARTESIAN_POINT ( 'NONE',  ( 4.999999999999998224, -44.99999999999997158, -97.79300000002184845 ) ) ;
#5280 = CARTESIAN_POINT ( 'NONE',  ( -38.82739432537914581, -32.55000000000000426, 1.398121909749243663 ) ) ;
#5281 = CARTESIAN_POINT ( 'NONE',  ( -24.64110105645932336, -7.999999999999996447, -24.00000000000000000 ) ) ;
#5282 = CIRCLE ( 'NONE', #1638, 2.099999999999997868 ) ;
#5283 = CARTESIAN_POINT ( 'NONE',  ( -28.51387258211773812, -46.80000000000001137, 9.383039235653802379 ) ) ;
#5284 = DIRECTION ( 'NONE',  ( 1.000000000000000000, 0.000000000000000000, 0.000000000000000000 ) ) ;
#5285 = ORIENTED_EDGE ( 'NONE', *, *, #8234, .F. ) ;
#5286 = CARTESIAN_POINT ( 'NONE',  ( 0.000000000000000000, 0.000000000000000000, 60.00000000000002842 ) ) ;
#5287 = CIRCLE ( 'NONE', #3485, 1.000000000000000888 ) ;
#5288 = CARTESIAN_POINT ( 'NONE',  ( -31.48612741788231517, -48.30000000000001137, -9.383039235653804155 ) ) ;
#5289 = CARTESIAN_POINT ( 'NONE',  ( -31.32969295284206979, -30.30000000000000782, -8.395350895058669494 ) ) ;
#5290 = DIRECTION ( 'NONE',  ( 0.000000000000000000, -0.5000000000000012212, -0.8660254037844380415 ) ) ;
#5291 = AXIS2_PLACEMENT_3D ( 'NONE', #7116, #1751, #1078 ) ;
#5292 = CARTESIAN_POINT ( 'NONE',  ( 34.96649286315892624, -44.33520523457834628, 11.47122145076291666 ) ) ;
#5293 = CARTESIAN_POINT ( 'NONE',  ( -28.49241082802385350, -40.44859572486944188, -9.874625247442173404 ) ) ;
#5294 = EDGE_CURVE ( 'NONE', #4697, #7212, #3494, .T. ) ;
#5295 = CARTESIAN_POINT ( 'NONE',  ( -26.64110105645932336, 8.000000000000000000, 124.0000000000000000 ) ) ;
#5296 = CYLINDRICAL_SURFACE ( 'NONE', #7515, 12.49999999999997691 ) ;
#5297 = CARTESIAN_POINT ( 'NONE',  ( -4.566987299999998307, -43.10829192115428299, -95.29999999890750928 ) ) ;
#5298 = AXIS2_PLACEMENT_3D ( 'NONE', #8206, #4893, #7570 ) ;
#5299 = FILL_AREA_STYLE ('',( #1381 ) ) ;
#5300 = ORIENTED_EDGE ( 'NONE', *, *, #5775, .F. ) ;
#5301 = CARTESIAN_POINT ( 'NONE',  ( -4.999999999999997335, -47.07106781186546129, -98.95000000000000284 ) ) ;
#5302 = CARTESIAN_POINT ( 'NONE',  ( -37.54950433343896776, -33.39859572486943762, 3.906122232810848249 ) ) ;
#5303 = CARTESIAN_POINT ( 'NONE',  ( -23.71967171589458445, -46.74859572486943904, -6.359104887540838469 ) ) ;
#5304 = CARTESIAN_POINT ( 'NONE',  ( -38.46456197978948666, -50.40000000000000568, 4.312909747525784709 ) ) ;
#5305 = AXIS2_PLACEMENT_3D ( 'NONE', #3189, #4997, #1645 ) ;
#5306 = EDGE_CURVE ( 'NONE', #2517, #505, #703, .T. ) ;
#5307 = ORIENTED_EDGE ( 'NONE', *, *, #2621, .T. ) ;
#5308 = ORIENTED_EDGE ( 'NONE', *, *, #1609, .F. ) ;
#5309 = CARTESIAN_POINT ( 'NONE',  ( -22.89739904353894318, -47.75140427513058938, -7.023824353025938549 ) ) ;
#5310 = CARTESIAN_POINT ( 'NONE',  ( 30.00000000000001421, -44.99999999999995737, 30.00000000000000000 ) ) ;
#5311 = DIRECTION ( 'NONE',  ( 0.000000000000000000, 0.000000000000000000, 1.000000000000000000 ) ) ;
#5312 = CARTESIAN_POINT ( 'NONE',  ( 2.071067811865477282, -49.99999999999996447, -99.44999999781505551 ) ) ;
#5313 = DIRECTION ( 'NONE',  ( 0.000000000000000000, -1.000000000000000000, 0.000000000000000000 ) ) ;
#5314 = CARTESIAN_POINT ( 'NONE',  ( 2.071067811865477282, -49.99999999999996447, -98.75000000000001421 ) ) ;
#5315 = ORIENTED_EDGE ( 'NONE', *, *, #1884, .F. ) ;
#5316 = CARTESIAN_POINT ( 'NONE',  ( -22.42644454439892598, -39.90000000000000568, -3.858919247786222861 ) ) ;
#5317 = CARTESIAN_POINT ( 'NONE',  ( -31.74999999999995737, 0.000000000000000000, 0.000000000000000000 ) ) ;
#5318 = EDGE_CURVE ( 'NONE', #3379, #5895, #3627, .T. ) ;
#5319 = VERTEX_POINT ( 'NONE', #1864 ) ;
#5320 = CARTESIAN_POINT ( 'NONE',  ( 4.566987299999998307, -44.99999999999997158, -99.04999999890752349 ) ) ;
#5321 = CARTESIAN_POINT ( 'NONE',  ( 4.999999999999998224, -44.99999999999997158, -99.40000000000000568 ) ) ;
#5322 = CARTESIAN_POINT ( 'NONE',  ( -31.56260684030781505, -43.95000000000000284, 9.865911304835510265 ) ) ;
#5323 = CARTESIAN_POINT ( 'NONE',  ( 1.891708078845685481, -49.56698729999997255, -97.39999999890751781 ) ) ;
#5324 = FILL_AREA_STYLE_COLOUR ( '', #6061 ) ;
#5325 = EDGE_CURVE ( 'NONE', #8403, #4829, #556, .T. ) ;
#5326 = CARTESIAN_POINT ( 'NONE',  ( -21.16389173201424612, -33.05140427513057233, -1.343104241417630185 ) ) ;
#5327 = CARTESIAN_POINT ( 'NONE',  ( 4.999999999999998224, -44.99999999999997158, -95.39300000002184277 ) ) ;
#5328 = CARTESIAN_POINT ( 'NONE',  ( -31.39812190974910422, -37.94999999999999574, 8.827394325379140483 ) ) ;
#5329 = CARTESIAN_POINT ( 'NONE',  ( -4.999999999999994671, -42.92893218813449607, -97.45000000000000284 ) ) ;
#5330 = CARTESIAN_POINT ( 'NONE',  ( -31.48612741788231517, -48.30000000000001137, -9.383039235653804155 ) ) ;
#5331 = ORIENTED_EDGE ( 'NONE', *, *, #5517, .T. ) ;
#5332 = DIRECTION ( 'NONE',  ( -0.000000000000000000, 1.000000000000000000, -0.000000000000000000 ) ) ;
#5333 = CARTESIAN_POINT ( 'NONE',  ( -22.93678734525658314, -45.74999999999999289, -7.063212654743582952 ) ) ;
#5334 = CARTESIAN_POINT ( 'NONE',  ( -22.42644454439892598, -30.90000000000000924, -3.858919247786222861 ) ) ;
#5335 = DIRECTION ( 'NONE',  ( 1.000000000000000000, 0.000000000000000000, 0.000000000000000000 ) ) ;
#5336 = DIRECTION ( 'NONE',  ( 0.000000000000000000, 0.000000000000000000, 1.000000000000000000 ) ) ;
#5337 = CARTESIAN_POINT ( 'NONE',  ( -31.53845232986046554, -40.29859572486944330, -9.374751783755117529 ) ) ;
#5338 = CARTESIAN_POINT ( 'NONE',  ( 10.00000000000000000, 1.224646799147353256E-15, 0.000000000000000000 ) ) ;
#5339 = DIRECTION ( 'NONE',  ( 0.000000000000000000, 0.000000000000000000, 1.000000000000000000 ) ) ;
#5340 = CARTESIAN_POINT ( 'NONE',  ( 8.389419568037416259E-16, -49.56698729999997255, -95.84999999890753486 ) ) ;
#5341 = CIRCLE ( 'NONE', #1282, 7.499999999999999112 ) ;
#5342 = ORIENTED_EDGE ( 'NONE', *, *, #8374, .F. ) ;
#5343 = DIRECTION ( 'NONE',  ( 0.000000000000000000, 0.000000000000000000, -1.000000000000000000 ) ) ;
#5344 = CARTESIAN_POINT ( 'NONE',  ( -38.40363834695740053, -33.69859572486942767, -1.277368040863739118 ) ) ;
#5345 = CARTESIAN_POINT ( 'NONE',  ( -28.46154767013959486, -41.79859572486943620, 9.374751783755112200 ) ) ;
#5346 = CARTESIAN_POINT ( 'NONE',  ( -20.12537475255788522, -39.05140427513057944, -1.507589171976365439 ) ) ;
#5347 = AXIS2_PLACEMENT_3D ( 'NONE', #2396, #973, #2926 ) ;
#5348 = ORIENTED_EDGE ( 'NONE', *, *, #5325, .F. ) ;
#5349 = ORIENTED_EDGE ( 'NONE', *, *, #5570, .T. ) ;
#5350 = CARTESIAN_POINT ( 'NONE',  ( -39.87462524744216807, -49.55140427513056522, 1.507589171976367215 ) ) ;
#5351 = CARTESIAN_POINT ( 'NONE',  ( 0.000000000000000000, 0.000000000000000000, 3.299999999999999822 ) ) ;
#5352 = CARTESIAN_POINT ( 'NONE',  ( 2.071067811865477282, -49.99999999999996447, -98.64999999781504414 ) ) ;
#5353 = CARTESIAN_POINT ( 'NONE',  ( 3.535533905932736420, -41.46446609406723383, -95.29999999999999716 ) ) ;
#5354 = PLANE ( 'NONE',  #83 ) ;
#5355 = ADVANCED_FACE ( 'NONE', ( #4348 ), #7825, .T. ) ;
#5356 = ORIENTED_EDGE ( 'NONE', *, *, #6223, .F. ) ;
#5357 =( GEOMETRIC_REPRESENTATION_CONTEXT ( 3 ) GLOBAL_UNCERTAINTY_ASSIGNED_CONTEXT ( ( #4064 ) ) GLOBAL_UNIT_ASSIGNED_CONTEXT ( ( #7121, #4518, #7872 ) ) REPRESENTATION_CONTEXT ( 'NONE', 'WORKASPACE' ) );
#5358 = CARTESIAN_POINT ( 'NONE',  ( -36.01040764008574513, -48.00000000000000711, -6.010407640085605685 ) ) ;
#5359 = CARTESIAN_POINT ( 'NONE',  ( -20.13408869516453947, -37.05000000000001137, -1.562606840307983136 ) ) ;
#5360 = AXIS2_PLACEMENT_3D ( 'NONE', #7685, #566, #7278 ) ;
#5361 = ORIENTED_EDGE ( 'NONE', *, *, #3375, .T. ) ;
#5362 = CARTESIAN_POINT ( 'NONE',  ( -4.566987299999997418, -46.89170807884566017, -99.39999999890751781 ) ) ;
#5363 = CARTESIAN_POINT ( 'NONE',  ( -3.535533905932736864, -41.46446609406723383, -96.59999999781504698 ) ) ;
#5364 = CARTESIAN_POINT ( 'NONE',  ( -21.09983283352784156, -40.35000000000000142, 4.534861676072186043 ) ) ;
#5365 = CARTESIAN_POINT ( 'NONE',  ( -3.229347689422840784, -41.77065231057713390, -97.74999999890752633 ) ) ;
#5366 = LINE ( 'NONE', #3361, #1554 ) ;
#5367 = CARTESIAN_POINT ( 'NONE',  ( -35.97294713907137975, -35.00140427513057517, -6.047868141099968398 ) ) ;
#5368 = EDGE_CURVE ( 'NONE', #2514, #1305, #7845, .T. ) ;
#5369 = CARTESIAN_POINT ( 'NONE',  ( -2.071067811865475505, -49.99999999999996447, -98.04300000002186266 ) ) ;
#5370 = CARTESIAN_POINT ( 'NONE',  ( -38.39535089505872634, -38.70000000000000284, -1.329692952841885267 ) ) ;
#5371 = DIRECTION ( 'NONE',  ( -1.000000000000000000, 0.000000000000000000, 0.000000000000000000 ) ) ;
#5372 = LINE ( 'NONE', #6743, #4975 ) ;
#5373 = EDGE_LOOP ( 'NONE', ( #2067, #279, #3869 ) ) ;
#5374 = DIRECTION ( 'NONE',  ( 1.000000000000000000, 0.000000000000000000, 0.000000000000000000 ) ) ;
#5375 = AXIS2_PLACEMENT_3D ( 'NONE', #3932, #4681, #7233 ) ;
#5376 = CARTESIAN_POINT ( 'NONE',  ( -38.90016716647221529, -47.85000000000000853, -4.534861676072185155 ) ) ;
#5377 = CARTESIAN_POINT ( 'NONE',  ( -22.06198138166579170, -45.35140427513057659, 4.107139971057695682 ) ) ;
#5378 = AXIS2_PLACEMENT_3D ( 'NONE', #5310, #5265, #7299 ) ;
#5379 = CARTESIAN_POINT ( 'NONE',  ( 33.61000000000001364, 0.000000000000000000, 2.000000000000000888 ) ) ;
#5380 = DIRECTION ( 'NONE',  ( -1.000000000000000000, -0.000000000000000000, -0.000000000000000000 ) ) ;
#5381 = CARTESIAN_POINT ( 'NONE',  ( -28.49241082802385350, -46.44859572486943478, -9.874625247442173404 ) ) ;
#5382 = VECTOR ( 'NONE', #3543, 1000.000000000000000 ) ;
#5383 = CARTESIAN_POINT ( 'NONE',  ( -4.999999999999998224, -44.99999999999997158, -99.69999999781505551 ) ) ;
#5384 = CARTESIAN_POINT ( 'NONE',  ( -1.891708078845683483, -49.56698729999997255, -96.69999999890755760 ) ) ;
#5385 = ORIENTED_EDGE ( 'NONE', *, *, #1418, .T. ) ;
#5386 = DIRECTION ( 'NONE',  ( 1.000000000000000000, 0.000000000000000000, 0.000000000000000000 ) ) ;
#5387 = EDGE_CURVE ( 'NONE', #5042, #112, #2364, .T. ) ;
#5388 = CARTESIAN_POINT ( 'NONE',  ( -38.39535089505872634, -47.70000000000000284, -1.329692952841885267 ) ) ;
#5389 = CARTESIAN_POINT ( 'NONE',  ( -38.92545601287626056, -42.84859572486944046, -4.485229520447501450 ) ) ;
#5390 = CARTESIAN_POINT ( 'NONE',  ( -25.63988726744978663, -41.60140427513058370, -8.440510857627391061 ) ) ;
#5391 = VECTOR ( 'NONE', #1877, 1000.000000000000000 ) ;
#5392 = ORIENTED_EDGE ( 'NONE', *, *, #1539, .F. ) ;
#5393 = VERTEX_POINT ( 'NONE', #1790 ) ;
#5394 = CARTESIAN_POINT ( 'NONE',  ( -34.48522952044771017, -41.15140427513058086, -8.925456012876139766 ) ) ;
#5395 = CARTESIAN_POINT ( 'NONE',  ( -49.99999999999997158, 60.00000000000002842, 30.00000000000000000 ) ) ;
#5396 = CARTESIAN_POINT ( 'NONE',  ( -20.00000000000002487, 0.000000000000000000, -45.00000000000000000 ) ) ;
#5397 = CARTESIAN_POINT ( 'NONE',  ( -4.999999999999997335, -47.07106781186546129, -98.84999999781503277 ) ) ;
#5398 = DIRECTION ( 'NONE',  ( -0.000000000000000000, -0.000000000000000000, 1.000000000000000000 ) ) ;
#5399 = CARTESIAN_POINT ( 'NONE',  ( -3.061616997868382155E-16, -39.99999999999997158, -100.0000000000000000 ) ) ;
#5400 = ORIENTED_EDGE ( 'NONE', *, *, #3664, .F. ) ;
#5401 = CARTESIAN_POINT ( 'NONE',  ( -23.71967171589458445, -31.74859572486943193, -6.359104887540838469 ) ) ;
#5402 = CARTESIAN_POINT ( 'NONE',  ( -38.90016716647221529, -32.85000000000000853, -4.534861676072185155 ) ) ;
#5403 = ORIENTED_EDGE ( 'NONE', *, *, #3019, .F. ) ;
#5404 = EDGE_CURVE ( 'NONE', #2540, #4041, #1159, .T. ) ;
#5405 = VERTEX_POINT ( 'NONE', #989 ) ;
#5406 = CARTESIAN_POINT ( 'NONE',  ( 4.566987299999998307, -43.10829192115428299, -97.39999999890753202 ) ) ;
#5407 = CARTESIAN_POINT ( 'NONE',  ( 5.000000000000000000, -47.07106781186545419, -97.74999999781503845 ) ) ;
#5408 = CARTESIAN_POINT ( 'NONE',  ( -28.51387258211773812, -40.80000000000000426, 9.383039235653802379 ) ) ;
#5409 = CARTESIAN_POINT ( 'NONE',  ( -1.891708078845683483, -49.56698729999997255, -99.09999999890753486 ) ) ;
#5410 = DIRECTION ( 'NONE',  ( -1.000000000000000000, 0.000000000000000000, -0.000000000000000000 ) ) ;
#5411 = CARTESIAN_POINT ( 'NONE',  ( -23.64089511245930098, -47.75140427513058938, -6.280328284105564762 ) ) ;
#5412 = EDGE_CURVE ( 'NONE', #8113, #4311, #6005, .T. ) ;
#5413 = CARTESIAN_POINT ( 'NONE',  ( 2.071067811865474173, -39.99999999999997158, -95.24300000002185129 ) ) ;
#5414 = CIRCLE ( 'NONE', #5985, 1.649999999999998579 ) ;
#5415 = CARTESIAN_POINT ( 'NONE',  ( -22.42644454439892598, -48.90000000000000568, -3.858919247786222861 ) ) ;
#5416 = CARTESIAN_POINT ( 'NONE',  ( 28.37383639613264208, -49.73950299483291104, 12.39754634550704182 ) ) ;
#5417 = DIRECTION ( 'NONE',  ( -0.000000000000000000, 1.000000000000000000, -0.000000000000000000 ) ) ;
#5418 = PRODUCT_CONTEXT ( 'NONE', #2741, 'mechanical' ) ;
#5419 = ORIENTED_EDGE ( 'NONE', *, *, #771, .F. ) ;
#5420 = PLANE ( 'NONE',  #1800 ) ;
#5421 = CARTESIAN_POINT ( 'NONE',  ( -28.43739315969223824, -45.45000000000000995, -9.865911304835512041 ) ) ;
#5422 = CARTESIAN_POINT ( 'NONE',  ( -35.97294713907137975, -50.00140427513058938, -6.047868141099968398 ) ) ;
#5423 = CIRCLE ( 'NONE', #6555, 2.149999999999985256 ) ;
#5424 = ADVANCED_FACE ( 'NONE', ( #3855 ), #483, .F. ) ;
#5425 = CARTESIAN_POINT ( 'NONE',  ( -25.25873964592378229, -43.37909215248190264, 11.56670877700491040 ) ) ;
#5426 = AXIS2_PLACEMENT_3D ( 'NONE', #5656, #1649, #2897 ) ;
#5427 = DIRECTION ( 'NONE',  ( 1.000000000000000000, 0.000000000000000000, 0.000000000000000000 ) ) ;
#5428 = CARTESIAN_POINT ( 'NONE',  ( -39.85719736222883824, -45.54859572486944330, 1.617624508639602388 ) ) ;
#5429 = CARTESIAN_POINT ( 'NONE',  ( 50.00000000000002842, -59.99999999999997158, -30.00000000000000000 ) ) ;
#5430 = CARTESIAN_POINT ( 'NONE',  ( 4.999999999999998224, -44.99999999999997158, -99.29999999781504982 ) ) ;
#5431 = ORIENTED_EDGE ( 'NONE', *, *, #6037, .F. ) ;
#5432 = FACE_OUTER_BOUND ( 'NONE', #4049, .T. ) ;
#5433 = CARTESIAN_POINT ( 'NONE',  ( -28.65689575858256077, -31.44859572486944188, -8.836108267985801845 ) ) ;
#5434 = CARTESIAN_POINT ( 'NONE',  ( -38.44051085762733777, -36.39859572486944472, 4.360112732550414982 ) ) ;
#5435 = CARTESIAN_POINT ( 'NONE',  ( -21.12512167993187973, -39.35140427513057659, 4.584493831696868860 ) ) ;
#5436 = EDGE_LOOP ( 'NONE', ( #8272, #6119 ) ) ;
#5437 = ORIENTED_EDGE ( 'NONE', *, *, #2472, .T. ) ;
#5438 = CARTESIAN_POINT ( 'NONE',  ( -21.51138689804841420, -44.90140427513058086, -4.265706762501151772 ) ) ;
#5439 = DIRECTION ( 'NONE',  ( 1.000000000000000000, -0.000000000000000000, -0.000000000000000000 ) ) ;
#5440 = CARTESIAN_POINT ( 'NONE',  ( -4.999999999999998224, -44.99999999999997158, -99.69999999781505551 ) ) ;
#5441 = DIRECTION ( 'NONE',  ( -0.000000000000000000, -1.000000000000000000, -0.000000000000000000 ) ) ;
#5442 = CARTESIAN_POINT ( 'NONE',  ( -25.00000000000002487, -45.00000000000000000, 11.45643923738959025 ) ) ;
#5443 = VERTEX_POINT ( 'NONE', #8487 ) ;
#5444 = VECTOR ( 'NONE', #7275, 1000.000000000000000 ) ;
#5445 = CARTESIAN_POINT ( 'NONE',  ( -38.39535089505872634, -47.70000000000000284, -1.329692952841885267 ) ) ;
#5446 = CARTESIAN_POINT ( 'NONE',  ( -36.71751442127229836, -39.00000000000000711, -6.717514421272142044 ) ) ;
#5447 = EDGE_LOOP ( 'NONE', ( #6774, #6994, #5928, #5901 ) ) ;
#5448 = DIRECTION ( 'NONE',  ( -1.000000000000000000, 0.000000000000000000, 0.000000000000000000 ) ) ;
#5449 = CARTESIAN_POINT ( 'NONE',  ( -2.796473189345805913E-16, -40.43301269999997061, -98.04999999890752349 ) ) ;
#5450 = CARTESIAN_POINT ( 'NONE',  ( 4.999999999999998224, -44.99999999999997158, -96.09999999781504698 ) ) ;
#5451 = LINE ( 'NONE', #964, #6225 ) ;
#5452 = CIRCLE ( 'NONE', #663, 3.500000000000000000 ) ;
#5453 = CARTESIAN_POINT ( 'NONE',  ( 8.389419568037416259E-16, -49.56698729999997255, -97.44999999890751496 ) ) ;
#5454 = ADVANCED_FACE ( 'NONE', ( #4390 ), #6366, .T. ) ;
#5455 = DIRECTION ( 'NONE',  ( -0.000000000000000000, 1.467581828789149532E-15, 1.000000000000000000 ) ) ;
#5456 = CARTESIAN_POINT ( 'NONE',  ( -37.59760657776328685, -40.40140427513058086, 3.811716262761598362 ) ) ;
#5457 = EDGE_CURVE ( 'NONE', #4453, #764, #3896, .T. ) ;
#5458 = CARTESIAN_POINT ( 'NONE',  ( 9.184850993605145972E-16, -49.99999999999997158, -95.59300000002185982 ) ) ;
#5459 = UNCERTAINTY_MEASURE_WITH_UNIT (LENGTH_MEASURE( 1.000000000000000082E-05 ), #974, 'distance_accuracy_value', 'NONE');
#5460 = CARTESIAN_POINT ( 'NONE',  ( -36.31971658582311591, -41.25000000000000711, 6.319716585823200283 ) ) ;
#5461 = CARTESIAN_POINT ( 'NONE',  ( -18.00000000000023093, 1.469576158976798506E-15, -44.00000000000000000 ) ) ;
#5462 = EDGE_CURVE ( 'NONE', #2812, #6772, #2894, .T. ) ;
#5463 = EDGE_LOOP ( 'NONE', ( #4728, #2406, #7595, #4913 ) ) ;
#5464 = FACE_OUTER_BOUND ( 'NONE', #6498, .T. ) ;
#5465 = CARTESIAN_POINT ( 'NONE',  ( -20.61696076434619584, -49.20000000000000995, 1.486127417882100676 ) ) ;
#5466 = CARTESIAN_POINT ( 'NONE',  ( -21.61293655684001536, -45.20140427513059223, 1.382017864820032971 ) ) ;
#5467 = CARTESIAN_POINT ( 'NONE',  ( 39.85000000000002274, -21.99999999999992184, 60.00000000000002842 ) ) ;
#5468 = EDGE_CURVE ( 'NONE', #4891, #4798, #7157, .T. ) ;
#5469 = DIRECTION ( 'NONE',  ( -0.000000000000000000, -0.000000000000000000, 1.000000000000000000 ) ) ;
#5470 = CARTESIAN_POINT ( 'NONE',  ( -31.53845232986046554, -46.29859572486944330, -9.374751783755117529 ) ) ;
#5471 = CARTESIAN_POINT ( 'NONE',  ( -7.654042494670954648E-16, -39.99999999999997158, -100.0000000000000000 ) ) ;
#5472 = CARTESIAN_POINT ( 'NONE',  ( -28.51387258211773812, -34.80000000000000426, 9.383039235653802379 ) ) ;
#5473 = ORIENTED_EDGE ( 'NONE', *, *, #2565, .F. ) ;
#5474 = LINE ( 'NONE', #6846, #6942 ) ;
#5475 = VERTEX_POINT ( 'NONE', #1117 ) ;
#5476 = CARTESIAN_POINT ( 'NONE',  ( -23.95213185889994989, -32.49859572486943904, 5.972947139071243861 ) ) ;
#5477 = EDGE_CURVE ( 'NONE', #5715, #8141, #96, .T. ) ;
#5478 = EDGE_CURVE ( 'NONE', #2602, #8290, #988, .T. ) ;
#5479 = CARTESIAN_POINT ( 'NONE',  ( -23.24502507771338600, -41.49859572486943904, 6.680053920257780220 ) ) ;
#5480 = CARTESIAN_POINT ( 'NONE',  ( -21.12512167993187973, -42.35140427513057659, 4.584493831696868860 ) ) ;
#5481 = CONICAL_SURFACE ( 'NONE', #7461, 12.49999999999996980, 1.029744258676651869 ) ;
#5482 = VERTEX_POINT ( 'NONE', #3984 ) ;
#5483 = ORIENTED_EDGE ( 'NONE', *, *, #2902, .F. ) ;
#5484 = CARTESIAN_POINT ( 'NONE',  ( -3.229347689422840784, -41.77065231057713390, -96.14999999890753202 ) ) ;
#5485 = CARTESIAN_POINT ( 'NONE',  ( 4.000000000000003553, 0.000000000000000000, 0.000000000000000000 ) ) ;
#5486 = CARTESIAN_POINT ( 'NONE',  ( -31.74999999999995737, 2.449293598294707893E-16, -2.000000000000000888 ) ) ;
#5487 = AXIS2_PLACEMENT_3D ( 'NONE', #5295, #3376, #8091 ) ;
#5488 = CARTESIAN_POINT ( 'NONE',  ( 4.566987299999998307, -43.10829192115428299, -97.39999999890751781 ) ) ;
#5489 = DIRECTION ( 'NONE',  ( -1.000000000000000000, 0.000000000000000000, 0.000000000000000000 ) ) ;
#5490 = CARTESIAN_POINT ( 'NONE',  ( 0.000000000000000000, 0.000000000000000000, 30.00000000000000000 ) ) ;
#5491 = EDGE_LOOP ( 'NONE', ( #3054, #6233 ) ) ;
#5492 = CARTESIAN_POINT ( 'NONE',  ( -23.68028341417693738, -48.75000000000001421, -6.319716585823198507 ) ) ;
#5493 = CARTESIAN_POINT ( 'NONE',  ( -34.53486167607238144, -33.15000000000001279, -8.900167166472096270 ) ) ;
#5494 = ORIENTED_EDGE ( 'NONE', *, *, #3230, .F. ) ;
#5495 = CARTESIAN_POINT ( 'NONE',  ( -34.53486167607238144, -45.14999999999999858, -8.900167166472096270 ) ) ;
#5496 = CARTESIAN_POINT ( 'NONE',  ( -4.999999999999998224, -44.99999999999997158, -98.89999999781504414 ) ) ;
#5497 = CARTESIAN_POINT ( 'NONE',  ( 3.229347689422839895, -41.77065231057713390, -98.14999999890751781 ) ) ;
#5498 = CARTESIAN_POINT ( 'NONE',  ( -4.999999999999998224, -44.99999999999997158, -100.4999999978150385 ) ) ;
#5499 = STYLED_ITEM ( 'NONE', ( #6693 ), #8634 ) ;
#5500 = CARTESIAN_POINT ( 'NONE',  ( -39.38303923565386100, -50.70000000000000995, -1.486127417882099788 ) ) ;
#5501 = CARTESIAN_POINT ( 'NONE',  ( -4.566987299999997418, -46.89170807884566727, -98.39999999890753202 ) ) ;
#5502 = EDGE_CURVE ( 'NONE', #6167, #8337, #1647, .T. ) ;
#5503 = CARTESIAN_POINT ( 'NONE',  ( -31.27736804086391942, -47.30140427513057944, -8.403638346957361449 ) ) ;
#5504 = COLOUR_RGB ( '', 0.09019608, 0.27058824, 0.51372549) ;
#5505 = CARTESIAN_POINT ( 'NONE',  ( 2.071067811865474173, -39.99999999999997158, -99.24300000002186550 ) ) ;
#5506 = CARTESIAN_POINT ( 'NONE',  ( -41.99999999999996447, 60.00000000000002842, -20.35000000000000142 ) ) ;
#5507 = CARTESIAN_POINT ( 'NONE',  ( -28.67030704715798350, -43.80000000000000426, 8.395350895058669494 ) ) ;
#5508 = AXIS2_PLACEMENT_3D ( 'NONE', #6528, #3191, #2575 ) ;
#5509 = DIRECTION ( 'NONE',  ( 0.000000000000000000, 0.000000000000000000, 1.000000000000000000 ) ) ;
#5510 = PRODUCT_CONTEXT ( 'NONE', #8587, 'mechanical' ) ;
#5511 = EDGE_LOOP ( 'NONE', ( #385, #1938, #6722 ) ) ;
#5512 = FACE_OUTER_BOUND ( 'NONE', #868, .T. ) ;
#5513 = CARTESIAN_POINT ( 'NONE',  ( -18.00000000000019185, 1.469576158976803042E-15, -29.65000000000000213 ) ) ;
#5514 = CARTESIAN_POINT ( 'NONE',  ( -23.68028341417693738, -36.75000000000000711, -6.319716585823198507 ) ) ;
#5515 =( BOUNDED_CURVE ( )  B_SPLINE_CURVE ( 2, ( #977, #3673, #8438, #5079, #3022, #5695, #7063, #3321, #6697, #7274, #2523, #7188, #4678, #5243, #2570, #1147, #7940, #5280, #3974, #3842, #4019, #5994, #7987, #1904, #3229, #4590, #4545, #7231, #8686, #1863, #1234, #5912, #7320, #1990, #6524, #1191, #2659, #2701, #3364, #1946, #7365, #8602, #5200, #3275, #6566, #473, #4631, #3931, #8560, #3886, #1273, #7896, #6607, #5328, #8076, #609, #6653, #519, #5370, #8030, #1319, #562, #3188, #5868, #657, #6038, #1144, #8647, #5954, #4501, #2613, #2173, #4107, #4903, #7408, #5460, #2834, #4861, #4812, #6741, #5553, #8168, #1366, #2131, #2083, #43, #4724, #2220, #2793, #91, #4065, #7496, #5507, #1498, #702, #1543, #8217, #7453, #2925, #1458, #4152, #4768, #1410, #6218, #8124, #6830, #748, #7537, #8259, #3407, #6785, #3540, #223, #882, #4193, #7582, #795, #3497, #6176, #6875, #5599, #837, #134, #6086, #3454, #182, #5415, #2880, #4238, #2036, #6918, #3583, #6130, #2747, #6265, #8431, #3710, #1102, #4989, #3915, #266 ),
 .UNSPECIFIED., .F., .T. ) 
 B_SPLINE_CURVE_WITH_KNOTS ( ( 3, 2, 2, 2, 2, 2, 2, 2, 2, 2, 2, 2, 2, 2, 2, 2, 2, 2, 2, 2, 2, 2, 2, 2, 2, 2, 2, 2, 2, 2, 2, 2, 2, 2, 2, 2, 2, 2, 2, 2, 2, 2, 2, 2, 2, 2, 2, 2, 2, 2, 2, 2, 2, 2, 2, 2, 2, 2, 2, 2, 2, 2, 2, 2, 2, 2, 2, 2, 2, 2, 3 ),
 ( 0.000000000000000000, 0.01428571428571428527, 0.02857142857142857054, 0.04285714285714285754, 0.05714285714285714107, 0.07142857142857142461, 0.08571428571428571508, 0.1000000000000000056, 0.1142857142857142821, 0.1285714285714285587, 0.1428571428571428492, 0.1571428571428571397, 0.1714285714285714302, 0.1857142857142857206, 0.2000000000000000111, 0.2142857142857142738, 0.2285714285714285643, 0.2428571428571428548, 0.2571428571428571175, 0.2714285714285714080, 0.2857142857142856984, 0.2999999999999999889, 0.3142857142857142794, 0.3285714285714285698, 0.3428571428571428603, 0.3571428571428571508, 0.3714285714285714413, 0.3857142857142857317, 0.4000000000000000222, 0.4142857142857143127, 0.4285714285714285476, 0.4428571428571428381, 0.4571428571428571286, 0.4714285714285714191, 0.4857142857142857095, 0.5000000000000000000, 0.5142857142857142350, 0.5285714285714285809, 0.5428571428571428159, 0.5571428571428571619, 0.5714285714285713969, 0.5857142857142857428, 0.5999999999999999778, 0.6142857142857143238, 0.6285714285714285587, 0.6428571428571429047, 0.6571428571428571397, 0.6714285714285713746, 0.6857142857142857206, 0.6999999999999999556, 0.7142857142857143016, 0.7285714285714285365, 0.7428571428571428825, 0.7571428571428571175, 0.7714285714285714635, 0.7857142857142856984, 0.8000000000000000444, 0.8142857142857142794, 0.8285714285714286254, 0.8428571428571428603, 0.8571428571428570953, 0.8714285714285714413, 0.8857142857142856762, 0.9000000000000000222, 0.9142857142857142572, 0.9285714285714286031, 0.9428571428571428381, 0.9571428571428571841, 0.9714285714285714191, 0.9857142857142857650, 1.000000000000000000 ),
 .UNSPECIFIED. ) 
 CURVE ( )  GEOMETRIC_REPRESENTATION_ITEM ( )  RATIONAL_B_SPLINE_CURVE ( ( 1.000000000000000000, 0.9510565162951535312, 1.000000000000000000, 0.9510565162951535312, 1.000000000000000000, 0.9510565162951535312, 1.000000000000000000, 0.9510565162951535312, 1.000000000000000000, 0.9510565162951535312, 1.000000000000000000, 0.9510565162951535312, 1.000000000000000000, 0.9510565162951535312, 1.000000000000000000, 0.9510565162951535312, 1.000000000000000000, 0.9510565162951535312, 1.000000000000000000, 0.9510565162951535312, 1.000000000000000000, 0.9510565162951535312, 1.000000000000000000, 0.9510565162951535312, 1.000000000000000000, 0.9510565162951535312, 1.000000000000000000, 0.9510565162951535312, 1.000000000000000000, 0.9510565162951535312, 1.000000000000000000, 0.9510565162951535312, 1.000000000000000000, 0.9510565162951535312, 1.000000000000000000, 0.9510565162951535312, 1.000000000000000000, 0.9510565162951535312, 1.000000000000000000, 0.9510565162951535312, 1.000000000000000000, 0.9510565162951535312, 1.000000000000000000, 0.9510565162951535312, 1.000000000000000000, 0.9510565162951535312, 1.000000000000000000, 0.9510565162951535312, 1.000000000000000000, 0.9510565162951535312, 1.000000000000000000, 0.9510565162951535312, 1.000000000000000000, 0.9510565162951535312, 1.000000000000000000, 0.9510565162951535312, 1.000000000000000000, 0.9510565162951535312, 1.000000000000000000, 0.9510565162951535312, 1.000000000000000000, 0.9510565162951535312, 1.000000000000000000, 0.9510565162951535312, 1.000000000000000000, 0.9510565162951535312, 1.000000000000000000, 0.9510565162951535312, 1.000000000000000000, 0.9510565162951535312, 1.000000000000000000, 0.9510565162951535312, 1.000000000000000000, 0.9510565162951535312, 1.000000000000000000, 0.9510565162951535312, 1.000000000000000000, 0.9510565162951535312, 1.000000000000000000, 0.9510565162951535312, 1.000000000000000000, 0.9510565162951535312, 1.000000000000000000, 0.9510565162951535312, 1.000000000000000000, 0.9510565162951535312, 1.000000000000000000, 0.9510565162951535312, 1.000000000000000000, 0.9510565162951535312, 1.000000000000000000, 0.9510565162951535312, 1.000000000000000000, 0.9510565162951535312, 1.000000000000000000, 0.9510565162951535312, 1.000000000000000000, 0.9510565162951535312, 1.000000000000000000, 0.9510565162951535312, 1.000000000000000000, 0.9510565162951535312, 1.000000000000000000, 0.9510565162951535312, 1.000000000000000000, 0.9510565162951535312, 1.000000000000000000, 0.9510565162951535312, 1.000000000000000000, 0.9510565162951535312, 1.000000000000000000, 0.9510565162951535312, 1.000000000000000000, 0.9510565162951535312, 1.000000000000000000, 0.9510565162951535312, 1.000000000000000000, 0.9510565162951535312, 1.000000000000000000, 0.9510565162951535312, 1.000000000000000000, 0.9510565162951535312, 1.000000000000000000, 0.9510565162951535312, 1.000000000000000000, 0.9510565162951535312, 1.000000000000000000, 0.9510565162951535312, 1.000000000000000000, 0.9510565162951535312, 1.000000000000000000, 0.9510565162951535312, 1.000000000000000000, 0.9510565162951535312, 1.000000000000000000, 0.9510565162951535312, 1.000000000000000000, 0.9510565162951535312, 1.000000000000000000, 0.9510565162951535312, 1.000000000000000000 ) ) 
 REPRESENTATION_ITEM ( '' )  );
#5516 = CARTESIAN_POINT ( 'NONE',  ( -25.44732502511945782, -42.92638634940919928, 11.64163759925511599 ) ) ;
#5517 = EDGE_CURVE ( 'NONE', #71, #7654, #4641, .T. ) ;
#5518 = DIRECTION ( 'NONE',  ( -0.000000000000000000, -0.000000000000000000, -1.000000000000000000 ) ) ;
#5519 = CARTESIAN_POINT ( 'NONE',  ( -21.07454398712378918, -50.34859572486944046, 4.485229520447505003 ) ) ;
#5520 = DIRECTION ( 'NONE',  ( 0.000000000000000000, 0.000000000000000000, -1.000000000000000000 ) ) ;
#5521 = CARTESIAN_POINT ( 'NONE',  ( 2.071067811865477282, -49.99999999999997158, -99.44999999781505551 ) ) ;
#5522 = AXIS2_PLACEMENT_3D ( 'NONE', #2467, #7217, #8425 ) ;
#5523 = ORIENTED_EDGE ( 'NONE', *, *, #4679, .F. ) ;
#5524 = DIRECTION ( 'NONE',  ( 0.000000000000000000, -0.000000000000000000, 1.000000000000000000 ) ) ;
#5525 = VERTEX_POINT ( 'NONE', #6664 ) ;
#5526 = AXIS2_PLACEMENT_3D ( 'NONE', #2682, #4615, #8053 ) ;
#5527 = CARTESIAN_POINT ( 'NONE',  ( -38.40363834695740053, -39.69859572486944188, -1.277368040863739118 ) ) ;
#5528 = CARTESIAN_POINT ( 'NONE',  ( -38.92545601287626056, -36.84859572486944046, -4.485229520447501450 ) ) ;
#5529 = CARTESIAN_POINT ( 'NONE',  ( -34.36011273255026310, -43.10140427513058370, 8.440510857627391061 ) ) ;
#5530 = ORIENTED_EDGE ( 'NONE', *, *, #1421, .F. ) ;
#5531 = CARTESIAN_POINT ( 'NONE',  ( -4.566987299999998307, -43.10829192115428299, -97.69999999890751496 ) ) ;
#5532 = AXIS2_PLACEMENT_3D ( 'NONE', #7207, #4440, #5844 ) ;
#5533 = CARTESIAN_POINT ( 'NONE',  ( 43.73819270004214843, -44.99999999999997158, 0.000000000000000000 ) ) ;
#5534 = DIRECTION ( 'NONE',  ( -1.000000000000000000, 0.000000000000000000, 0.000000000000000000 ) ) ;
#5535 = CARTESIAN_POINT ( 'NONE',  ( -4.566987299999998307, -43.10829192115428299, -97.89999999890751781 ) ) ;
#5536 = DIRECTION ( 'NONE',  ( -1.000000000000000000, 0.000000000000000000, 0.000000000000000000 ) ) ;
#5537 = FACE_OUTER_BOUND ( 'NONE', #614, .T. ) ;
#5538 = ORIENTED_EDGE ( 'NONE', *, *, #5756, .F. ) ;
#5539 = CARTESIAN_POINT ( 'NONE',  ( -38.40363834695740053, -36.69859572486944188, -1.277368040863739118 ) ) ;
#5540 = CARTESIAN_POINT ( 'NONE',  ( -37.06321265474346660, -32.25000000000000711, 7.063212654743582952 ) ) ;
#5541 = ORIENTED_EDGE ( 'NONE', *, *, #6794, .F. ) ;
#5542 = CARTESIAN_POINT ( 'NONE',  ( -21.53543802021056663, -48.90000000000000568, -4.312909747525783821 ) ) ;
#5543 = CARTESIAN_POINT ( 'NONE',  ( -30.00000000000000000, 60.00000000000002842, 0.000000000000000000 ) ) ;
#5544 = CARTESIAN_POINT ( 'NONE',  ( -4.566987299999998307, -44.99999999999997158, -100.2499999989075121 ) ) ;
#5545 = CIRCLE ( 'NONE', #6955, 2.200000000000001066 ) ;
#5546 = CARTESIAN_POINT ( 'NONE',  ( 9.184850993605145972E-16, -49.99999999999997158, -99.49999999781503845 ) ) ;
#5547 = CARTESIAN_POINT ( 'NONE',  ( 50.00000000000002842, -59.99999999999997158, 30.00000000000000000 ) ) ;
#5548 = CARTESIAN_POINT ( 'NONE',  ( 4.566987299999998307, -44.99999999999997158, -97.24999999890752633 ) ) ;
#5549 = CARTESIAN_POINT ( 'NONE',  ( -33.90612223281073057, -40.10140427513057659, 7.549504333439023718 ) ) ;
#5550 = CARTESIAN_POINT ( 'NONE',  ( 9.184850993605145972E-16, -49.99999999999997158, -95.60000000000000853 ) ) ;
#5551 = UNCERTAINTY_MEASURE_WITH_UNIT (LENGTH_MEASURE( 1.000000000000000082E-05 ), #7150, 'distance_accuracy_value', 'NONE');
#5552 = CARTESIAN_POINT ( 'NONE',  ( 1.891708078845685481, -49.56698729999997255, -96.59999999890754907 ) ) ;
#5553 = CARTESIAN_POINT ( 'NONE',  ( -36.01040764008574513, -42.00000000000000711, -6.010407640085605685 ) ) ;
#5554 = CYLINDRICAL_SURFACE ( 'NONE', #4991, 1.000000000000000888 ) ;
#5555 = PRODUCT_CONTEXT ( 'NONE', #3360, 'mechanical' ) ;
#5556 = CARTESIAN_POINT ( 'NONE',  ( 5.000000000000000000, -47.07106781186545419, -100.1499999978150441 ) ) ;
#5557 = CARTESIAN_POINT ( 'NONE',  ( -31.32969295284206979, -42.30000000000000426, -8.395350895058669494 ) ) ;
#5558 = CARTESIAN_POINT ( 'NONE',  ( -28.37672147103137732, -40.25949688271495575, 12.39792973884354232 ) ) ;
#5559 = DIRECTION ( 'NONE',  ( -0.000000000000000000, 1.000000000000000000, -0.000000000000000000 ) ) ;
#5560 = CARTESIAN_POINT ( 'NONE',  ( -37.02382435302582309, -45.24859572486943904, 7.102600956461226467 ) ) ;
#5561 = DIRECTION ( 'NONE',  ( 0.000000000000000000, 1.000000000000000000, -1.467581828789149335E-15 ) ) ;
#5562 = DIRECTION ( 'NONE',  ( 1.000000000000000000, 0.000000000000000000, 0.000000000000000000 ) ) ;
#5563 = ORIENTED_EDGE ( 'NONE', *, *, #2044, .F. ) ;
#5564 = PLANE ( 'NONE',  #4178 ) ;
#5565 = ORIENTED_EDGE ( 'NONE', *, *, #1671, .F. ) ;
#5566 = CARTESIAN_POINT ( 'NONE',  ( -23.71967171589458445, -43.74859572486943904, -6.359104887540838469 ) ) ;
#5567 = CARTESIAN_POINT ( 'NONE',  ( -21.55948914237271907, -46.89859572486944472, -4.360112732550413206 ) ) ;
#5568 = CARTESIAN_POINT ( 'NONE',  ( -22.40239342223677355, -29.90140427513058796, -3.811716262761597473 ) ) ;
#5569 =( BOUNDED_SURFACE ( )  B_SPLINE_SURFACE ( 3, 2, ( 
 ( #168, #4140, #6905, #6204, #6819, #1485, #3526, #6166, #2732, #2690, #2024, #122, #2070, #4890, #2866, #5540, #8158, #73, #8246, #5402, #6862, #5493, #7441, #8203, #4052, #1399, #781, #3353, #2821, #6073, #691, #2205, #3484, #2161, #4847, #7567, #7526, #4180, #1352, #6029, #1528, #4095, #6732, #826, #4222, #2117, #7768, #5359, #8061, #4714, #31, #7397, #2781, #6771, #3397, #8111, #4756, #736, #3441, #6118, #5446, #4800, #7482, #1446, #3568, #6290, #2997, #2249, #7657, #6331, #2292, #7611, #8376, #2954, #209, #7037, #295, #4928, #914, #3695, #4267, #5672, #8418, #4442, #5717, #336, #6950, #1760, #997, #6375, #6253, #252, #1045, #8289, #1573, #5582, #3609, #5628, #8328, #1665, #2336, #8458, #375, #5017, #2912, #7706, #1711, #5760, #4974, #6993, #1619, #957, #4310, #3653, #4357, #3042, #867, #2382, #4398, #5057, #7747, #7087, #3737, #6418, #3083, #7791, #2421, #5101, #1922, #5182, #5804, #412, #8578, #7250, #1964, #1842, #5304, #1086, #1799, #1212, #5893 ),
 ( #6585, #4481, #8007, #4568, #3907, #3783, #3820, #7295, #8498, #7834, #3124, #7167, #6500, #2460, #7919, #6543, #5974, #6626, #3866, #5142, #2544, #7960, #3300, #3170, #4523, #6460, #7209, #1127, #1170, #453, #5846, #7125, #494, #4610, #1883, #3208, #8537, #540, #3251, #7876, #2504, #5221, #5931, #1252, #8624, #2592, #5261, #3950, #584, #8666, #2633, #4039, #3995, #3339, #7470, #3383, #6193, #1475, #7514, #721, #1386, #6850, #6719, #8189, #6808, #19, #769, #5346, #2720, #5435, #4652, #1431, #7386, #2011, #4169, #2105, #3472, #4127, #815, #6153, #111, #2677, #7339, #4835, #5390, #8049, #2809, #4787, #3429, #5480, #1295, #3516, #8145, #1340, #5529, #4082, #8099, #2149, #156, #2853, #4701, #8233, #6675, #678, #631, #6017, #8705, #6059, #2057, #6758, #4743, #7429, #6103, #63, #2767, #7598, #8363, #7025, #4345, #7075, #239, #1607, #7555, #4918, #986, #3684, #5703, #6322, #1562, #6239, #1518, #3600, #6364, #6280, #6893, #4297, #3726, #4211, #3072, #6408, #2942 ),
 ( #2901, #856, #5617, #945, #285, #8318, #5568, #8275, #5749, #3555, #6981, #1698, #3641, #2986, #1034, #2281, #326, #199, #5661, #7736, #2192, #2326, #5004, #7692, #1653, #363, #3032, #8406, #4962, #902, #7644, #2239, #4256, #2370, #6939, #5046, #4388, #4878, #6573, #1241, #526, #6489, #4431, #5208, #3110, #401, #7196, #7863, #1156, #8567, #3284, #3159, #6615, #2409, #5790, #2531, #3850, #2450, #8523, #5919, #7822, #570, #8447, #5088, #6449, #5171, #8485, #1075, #5131, #7778, #5878, #3237, #4598, #6532, #480, #5834, #440, #3937, #3195, #2580, #1748, #2489, #7904, #1871, #1828, #7113, #8609, #5250, #4554, #3768, #7947, #7282, #1787, #4469, #7154, #7238, #1115, #3807, #4509, #1198, #3894, #1910, #665, #6661, #617, #804, #7326, #8085, #5466, #5377, #4071, #4819, #6704, #1419, #4638, #2043, #2797, #5961, #4731, #7416, #2755, #1374, #7502, #7460, #710, #3371, #4687, #6045, #6002, #8693, #4114, #3328, #6747, #3982, #2666, #6793, #1463, #757, #4027, #1953, #5422 ),
 ( #3415, #8037, #5289, #6093, #2708, #1281, #5334, #51, #2620, #7, #3460, #1997, #6836, #8655, #7995, #7372, #8132, #1326, #2092, #4775, #6138, #98, #8175, #2138, #4158, #2269, #887, #4242, #7725, #4285, #6352, #142, #6924, #6967, #3628, #6268, #8223, #7012, #314, #934, #7059, #3018, #2356, #5035, #2841, #5514, #270, #3504, #185, #6309, #8348, #5648, #8393, #1547, #2929, #2180, #6224, #2314, #4992, #975, #7629, #2888, #7542, #4867, #4905, #7675, #7587, #1505, #5603, #1684, #4200, #4374, #6182, #3588, #6880, #843, #5693, #1640, #2972, #4333, #3670, #1592, #5557, #3544, #8263, #227, #2225, #8306, #4948, #5738, #4419, #1020, #3713, #6396, #8435, #352, #3060, #2398, #5075, #7765, #1733, #5971, #2009, #8097, #4741, #4036, #1292, #3993, #4167, #1962, #2718, #109, #17, #7427, #8187, #1338, #4785, #8005, #5388, #6151, #582, #2055, #1384, #6101, #4080, #2147, #2102, #6756, #6717, #8047, #675, #628, #3337, #7468, #6673, #719, #7337, #6015, #1429, #4833, #4125 ),
 ( #3427, #61, #2765, #5433, #3298, #3381, #7512, #8664, #8703, #6057, #5476, #2631, #7384, #6806, #2675, #1473, #5302, #4650, #5344, #8143, #4699, #767, #3470, #2807, #4295, #1651, #3030, #2279, #5615, #4254, #7596, #2368, #7642, #984, #3514, #1559, #1605, #6978, #900, #2851, #4343, #3681, #943, #1696, #6361, #5701, #8404, #6191, #153, #3639, #6848, #3553, #6320, #2984, #283, #5044, #4916, #6277, #5527, #854, #5658, #2899, #6937, #8231, #3598, #2190, #237, #6890, #4876, #813, #2940, #7023, #8361, #8316, #7553, #2324, #5002, #4959, #7734, #1516, #6237, #324, #7689, #4209, #197, #5566, #8273, #2236, #7194, #3765, #3724, #3070, #1153, #3108, #5917, #1196, #7236, #437, #1113, #6571, #6447, #7902, #6530, #8482, #478, #5086, #2448, #5168, #4386, #3848, #7111, #1746, #3892, #1826, #3193, #5876, #524, #8565, #2529, #2407, #7072, #4552, #5129, #7775, #5206, #4507, #3157, #1868, #1032, #3235, #7861, #1073, #5248, #3805, #7820, #8607, #2577, #7945, #4429, #6406, #361 ),
 ( #1785, #5747, #8445, #399, #5788, #5832, #6487, #8521, #4467, #7152, #2487, #573, #1956, #574, #2001, #6618, #1285, #5965, #7158, #3289, #8658, #1831, #8040, #4602, #7285, #3811, #3856, #7330, #5837, #7867, #3163, #4513, #6535, #8527, #7951, #6576, #6007, #6665, #3898, #444, #2583, #7999, #3330, #1161, #6493, #1244, #4642, #8696, #5253, #5923, #4559, #7908, #2669, #1914, #3985, #2493, #1874, #3941, #2624, #1203, #5174, #621, #5337, #5293, #1118, #7200, #484, #3200, #5883, #8570, #2534, #5213, #7242, #530, #3241, #8614, #847, #2758, #4118, #1329, #7422, #3508, #6185, #8227, #103, #1377, #11, #4031, #6096, #6840, #55, #669, #6799, #6228, #6709, #5560, #190, #5428, #7378, #2891, #1510, #146, #5470, #5381, #3374, #8137, #3463, #2800, #2096, #8090, #2047, #8267, #6049, #760, #4203, #6144, #8179, #3547, #4778, #2844, #2711, #2142, #6884, #4692, #4824, #7505, #1467, #4160, #4735, #5519, #807, #7464, #3420, #1423, #4074, #6751, #2183, #713, #4871, #7546, #8309 ),
 ( #7729, #5606, #2933, #978, #1644, #3674, #2360, #5907, #3592, #5038, #4909, #892, #4996, #7107, #7590, #274, #8439, #1597, #3225, #2230, #1552, #230, #7680, #2272, #6271, #4246, #2317, #4953, #7633, #6928, #4336, #5742, #3023, #7015, #4288, #8398, #1689, #2976, #513, #6972, #937, #2403, #5652, #3631, #6313, #5696, #357, #5080, #4379, #8353, #6355, #318, #7064, #1025, #3881, #7770, #1739, #3718, #6401, #4423, #3065, #1068, #6560, #3967, #2030, #555, #6644, #649, #8595, #5364, #2607, #5947, #5408, #6033, #4718, #8067, #2075, #7402, #2696, #6600, #2560, #36, #601, #3267, #1357, #4951, #7358, #4057, #5237, #8117, #3358, #5275, #742, #5322, #3315, #695, #6736, #3401, #8641, #6078, #2739, #7979, #4762, #7446, #1404, #7932, #1941, #1983, #1228, #5989, #8022, #1267, #4626, #1312, #7310, #8680, #4012, #6777, #4100, #3447, #1899, #4583, #7267, #3925, #2653, #4670, #6691, #788, #7001, #3576, #6260, #2786, #2827, #6297, #4806, #6824, #2123, #3490, #5500, #7488, #6912 ) ),
 .UNSPECIFIED., .T., .F., .T. ) 
 B_SPLINE_SURFACE_WITH_KNOTS ( ( 4, 3, 4 ),
 ( 3, 2, 2, 2, 2, 2, 2, 2, 2, 2, 2, 2, 2, 2, 2, 2, 2, 2, 2, 2, 2, 2, 2, 2, 2, 2, 2, 2, 2, 2, 2, 2, 2, 2, 2, 2, 2, 2, 2, 2, 2, 2, 2, 2, 2, 2, 2, 2, 2, 2, 2, 2, 2, 2, 2, 2, 2, 2, 2, 2, 2, 2, 2, 2, 2, 2, 2, 2, 2, 2, 3 ),
 ( 0.000000000000000000, 0.5000000000000000000, 1.000000000000000000 ),
 ( 0.000000000000000000, 0.01428571428571428527, 0.02857142857142857054, 0.04285714285714285754, 0.05714285714285714107, 0.07142857142857142461, 0.08571428571428571508, 0.1000000000000000056, 0.1142857142857142821, 0.1285714285714285587, 0.1428571428571428492, 0.1571428571428571397, 0.1714285714285714302, 0.1857142857142857206, 0.2000000000000000111, 0.2142857142857142738, 0.2285714285714285643, 0.2428571428571428548, 0.2571428571428571175, 0.2714285714285714080, 0.2857142857142856984, 0.2999999999999999889, 0.3142857142857142794, 0.3285714285714285698, 0.3428571428571428603, 0.3571428571428571508, 0.3714285714285714413, 0.3857142857142857317, 0.4000000000000000222, 0.4142857142857143127, 0.4285714285714285476, 0.4428571428571428381, 0.4571428571428571286, 0.4714285714285714191, 0.4857142857142857095, 0.5000000000000000000, 0.5142857142857142350, 0.5285714285714285809, 0.5428571428571428159, 0.5571428571428571619, 0.5714285714285713969, 0.5857142857142857428, 0.5999999999999999778, 0.6142857142857143238, 0.6285714285714285587, 0.6428571428571429047, 0.6571428571428571397, 0.6714285714285713746, 0.6857142857142857206, 0.6999999999999999556, 0.7142857142857143016, 0.7285714285714285365, 0.7428571428571428825, 0.7571428571428571175, 0.7714285714285714635, 0.7857142857142856984, 0.8000000000000000444, 0.8142857142857142794, 0.8285714285714286254, 0.8428571428571428603, 0.8571428571428570953, 0.8714285714285714413, 0.8857142857142856762, 0.9000000000000000222, 0.9142857142857142572, 0.9285714285714286031, 0.9428571428571428381, 0.9571428571428571841, 0.9714285714285714191, 0.9857142857142857650, 1.000000000000000000 ),
 .UNSPECIFIED. ) 
 GEOMETRIC_REPRESENTATION_ITEM ( )  RATIONAL_B_SPLINE_SURFACE ( (
 ( 1.000000000000000000, 0.9510565162951535312, 1.000000000000000000, 0.9510565162951535312, 1.000000000000000000, 0.9510565162951535312, 1.000000000000000000, 0.9510565162951535312, 1.000000000000000000, 0.9510565162951535312, 1.000000000000000000, 0.9510565162951535312, 1.000000000000000000, 0.9510565162951535312, 1.000000000000000000, 0.9510565162951535312, 1.000000000000000000, 0.9510565162951535312, 1.000000000000000000, 0.9510565162951535312, 1.000000000000000000, 0.9510565162951535312, 1.000000000000000000, 0.9510565162951535312, 1.000000000000000000, 0.9510565162951535312, 1.000000000000000000, 0.9510565162951535312, 1.000000000000000000, 0.9510565162951535312, 1.000000000000000000, 0.9510565162951535312, 1.000000000000000000, 0.9510565162951535312, 1.000000000000000000, 0.9510565162951535312, 1.000000000000000000, 0.9510565162951535312, 1.000000000000000000, 0.9510565162951535312, 1.000000000000000000, 0.9510565162951535312, 1.000000000000000000, 0.9510565162951535312, 1.000000000000000000, 0.9510565162951535312, 1.000000000000000000, 0.9510565162951535312, 1.000000000000000000, 0.9510565162951535312, 1.000000000000000000, 0.9510565162951535312, 1.000000000000000000, 0.9510565162951535312, 1.000000000000000000, 0.9510565162951535312, 1.000000000000000000, 0.9510565162951535312, 1.000000000000000000, 0.9510565162951535312, 1.000000000000000000, 0.9510565162951535312, 1.000000000000000000, 0.9510565162951535312, 1.000000000000000000, 0.9510565162951535312, 1.000000000000000000, 0.9510565162951535312, 1.000000000000000000, 0.9510565162951535312, 1.000000000000000000, 0.9510565162951535312, 1.000000000000000000, 0.9510565162951535312, 1.000000000000000000, 0.9510565162951535312, 1.000000000000000000, 0.9510565162951535312, 1.000000000000000000, 0.9510565162951535312, 1.000000000000000000, 0.9510565162951535312, 1.000000000000000000, 0.9510565162951535312, 1.000000000000000000, 0.9510565162951535312, 1.000000000000000000, 0.9510565162951535312, 1.000000000000000000, 0.9510565162951535312, 1.000000000000000000, 0.9510565162951535312, 1.000000000000000000, 0.9510565162951535312, 1.000000000000000000, 0.9510565162951535312, 1.000000000000000000, 0.9510565162951535312, 1.000000000000000000, 0.9510565162951535312, 1.000000000000000000, 0.9510565162951535312, 1.000000000000000000, 0.9510565162951535312, 1.000000000000000000, 0.9510565162951535312, 1.000000000000000000, 0.9510565162951535312, 1.000000000000000000, 0.9510565162951535312, 1.000000000000000000, 0.9510565162951535312, 1.000000000000000000, 0.9510565162951535312, 1.000000000000000000, 0.9510565162951535312, 1.000000000000000000, 0.9510565162951535312, 1.000000000000000000, 0.9510565162951535312, 1.000000000000000000, 0.9510565162951535312, 1.000000000000000000, 0.9510565162951535312, 1.000000000000000000, 0.9510565162951535312, 1.000000000000000000, 0.9510565162951535312, 1.000000000000000000, 0.9510565162951535312, 1.000000000000000000, 0.9510565162951535312, 1.000000000000000000, 0.9510565162951535312, 1.000000000000000000, 0.9510565162951535312, 1.000000000000000000, 0.9510565162951535312, 1.000000000000000000, 0.9510565162951535312, 1.000000000000000000),
 ( 0.3333333333333333703, 0.3170188387650512141, 0.3333333333333333703, 0.3170188387650512141, 0.3333333333333333703, 0.3170188387650512141, 0.3333333333333333703, 0.3170188387650512141, 0.3333333333333333703, 0.3170188387650512141, 0.3333333333333333703, 0.3170188387650512141, 0.3333333333333333703, 0.3170188387650512141, 0.3333333333333333703, 0.3170188387650512141, 0.3333333333333333703, 0.3170188387650512141, 0.3333333333333333703, 0.3170188387650512141, 0.3333333333333333703, 0.3170188387650512141, 0.3333333333333333703, 0.3170188387650512141, 0.3333333333333333703, 0.3170188387650512141, 0.3333333333333333703, 0.3170188387650512141, 0.3333333333333333703, 0.3170188387650512141, 0.3333333333333333703, 0.3170188387650512141, 0.3333333333333333703, 0.3170188387650512141, 0.3333333333333333703, 0.3170188387650512141, 0.3333333333333333703, 0.3170188387650512141, 0.3333333333333333703, 0.3170188387650512141, 0.3333333333333333703, 0.3170188387650512141, 0.3333333333333333703, 0.3170188387650512141, 0.3333333333333333703, 0.3170188387650512141, 0.3333333333333333703, 0.3170188387650512141, 0.3333333333333333703, 0.3170188387650512141, 0.3333333333333333703, 0.3170188387650512141, 0.3333333333333333703, 0.3170188387650512141, 0.3333333333333333703, 0.3170188387650512141, 0.3333333333333333703, 0.3170188387650512141, 0.3333333333333333703, 0.3170188387650512141, 0.3333333333333333703, 0.3170188387650512141, 0.3333333333333333703, 0.3170188387650512141, 0.3333333333333333703, 0.3170188387650512141, 0.3333333333333333703, 0.3170188387650512141, 0.3333333333333333703, 0.3170188387650512141, 0.3333333333333333703, 0.3170188387650512141, 0.3333333333333333703, 0.3170188387650512141, 0.3333333333333333703, 0.3170188387650512141, 0.3333333333333333703, 0.3170188387650512141, 0.3333333333333333703, 0.3170188387650512141, 0.3333333333333333703, 0.3170188387650512141, 0.3333333333333333703, 0.3170188387650512141, 0.3333333333333333703, 0.3170188387650512141, 0.3333333333333333703, 0.3170188387650512141, 0.3333333333333333703, 0.3170188387650512141, 0.3333333333333333703, 0.3170188387650512141, 0.3333333333333333703, 0.3170188387650512141, 0.3333333333333333703, 0.3170188387650512141, 0.3333333333333333703, 0.3170188387650512141, 0.3333333333333333703, 0.3170188387650512141, 0.3333333333333333703, 0.3170188387650512141, 0.3333333333333333703, 0.3170188387650512141, 0.3333333333333333703, 0.3170188387650512141, 0.3333333333333333703, 0.3170188387650512141, 0.3333333333333333703, 0.3170188387650512141, 0.3333333333333333703, 0.3170188387650512141, 0.3333333333333333703, 0.3170188387650512141, 0.3333333333333333703, 0.3170188387650512141, 0.3333333333333333703, 0.3170188387650512141, 0.3333333333333333703, 0.3170188387650512141, 0.3333333333333333703, 0.3170188387650512141, 0.3333333333333333703, 0.3170188387650512141, 0.3333333333333333703, 0.3170188387650512141, 0.3333333333333333703, 0.3170188387650512141, 0.3333333333333333703, 0.3170188387650512141, 0.3333333333333333703, 0.3170188387650512141, 0.3333333333333333703, 0.3170188387650512141, 0.3333333333333333703, 0.3170188387650512141, 0.3333333333333333703, 0.3170188387650512141, 0.3333333333333333703, 0.3170188387650512141, 0.3333333333333333703),
 ( 0.3333333333333333703, 0.3170188387650512141, 0.3333333333333333703, 0.3170188387650512141, 0.3333333333333333703, 0.3170188387650512141, 0.3333333333333333703, 0.3170188387650512141, 0.3333333333333333703, 0.3170188387650512141, 0.3333333333333333703, 0.3170188387650512141, 0.3333333333333333703, 0.3170188387650512141, 0.3333333333333333703, 0.3170188387650512141, 0.3333333333333333703, 0.3170188387650512141, 0.3333333333333333703, 0.3170188387650512141, 0.3333333333333333703, 0.3170188387650512141, 0.3333333333333333703, 0.3170188387650512141, 0.3333333333333333703, 0.3170188387650512141, 0.3333333333333333703, 0.3170188387650512141, 0.3333333333333333703, 0.3170188387650512141, 0.3333333333333333703, 0.3170188387650512141, 0.3333333333333333703, 0.3170188387650512141, 0.3333333333333333703, 0.3170188387650512141, 0.3333333333333333703, 0.3170188387650512141, 0.3333333333333333703, 0.3170188387650512141, 0.3333333333333333703, 0.3170188387650512141, 0.3333333333333333703, 0.3170188387650512141, 0.3333333333333333703, 0.3170188387650512141, 0.3333333333333333703, 0.3170188387650512141, 0.3333333333333333703, 0.3170188387650512141, 0.3333333333333333703, 0.3170188387650512141, 0.3333333333333333703, 0.3170188387650512141, 0.3333333333333333703, 0.3170188387650512141, 0.3333333333333333703, 0.3170188387650512141, 0.3333333333333333703, 0.3170188387650512141, 0.3333333333333333703, 0.3170188387650512141, 0.3333333333333333703, 0.3170188387650512141, 0.3333333333333333703, 0.3170188387650512141, 0.3333333333333333703, 0.3170188387650512141, 0.3333333333333333703, 0.3170188387650512141, 0.3333333333333333703, 0.3170188387650512141, 0.3333333333333333703, 0.3170188387650512141, 0.3333333333333333703, 0.3170188387650512141, 0.3333333333333333703, 0.3170188387650512141, 0.3333333333333333703, 0.3170188387650512141, 0.3333333333333333703, 0.3170188387650512141, 0.3333333333333333703, 0.3170188387650512141, 0.3333333333333333703, 0.3170188387650512141, 0.3333333333333333703, 0.3170188387650512141, 0.3333333333333333703, 0.3170188387650512141, 0.3333333333333333703, 0.3170188387650512141, 0.3333333333333333703, 0.3170188387650512141, 0.3333333333333333703, 0.3170188387650512141, 0.3333333333333333703, 0.3170188387650512141, 0.3333333333333333703, 0.3170188387650512141, 0.3333333333333333703, 0.3170188387650512141, 0.3333333333333333703, 0.3170188387650512141, 0.3333333333333333703, 0.3170188387650512141, 0.3333333333333333703, 0.3170188387650512141, 0.3333333333333333703, 0.3170188387650512141, 0.3333333333333333703, 0.3170188387650512141, 0.3333333333333333703, 0.3170188387650512141, 0.3333333333333333703, 0.3170188387650512141, 0.3333333333333333703, 0.3170188387650512141, 0.3333333333333333703, 0.3170188387650512141, 0.3333333333333333703, 0.3170188387650512141, 0.3333333333333333703, 0.3170188387650512141, 0.3333333333333333703, 0.3170188387650512141, 0.3333333333333333703, 0.3170188387650512141, 0.3333333333333333703, 0.3170188387650512141, 0.3333333333333333703, 0.3170188387650512141, 0.3333333333333333703, 0.3170188387650512141, 0.3333333333333333703, 0.3170188387650512141, 0.3333333333333333703, 0.3170188387650512141, 0.3333333333333333703, 0.3170188387650512141, 0.3333333333333333703),
 ( 1.000000000000000000, 0.9510565162951535312, 1.000000000000000000, 0.9510565162951535312, 1.000000000000000000, 0.9510565162951535312, 1.000000000000000000, 0.9510565162951535312, 1.000000000000000000, 0.9510565162951535312, 1.000000000000000000, 0.9510565162951535312, 1.000000000000000000, 0.9510565162951535312, 1.000000000000000000, 0.9510565162951535312, 1.000000000000000000, 0.9510565162951535312, 1.000000000000000000, 0.9510565162951535312, 1.000000000000000000, 0.9510565162951535312, 1.000000000000000000, 0.9510565162951535312, 1.000000000000000000, 0.9510565162951535312, 1.000000000000000000, 0.9510565162951535312, 1.000000000000000000, 0.9510565162951535312, 1.000000000000000000, 0.9510565162951535312, 1.000000000000000000, 0.9510565162951535312, 1.000000000000000000, 0.9510565162951535312, 1.000000000000000000, 0.9510565162951535312, 1.000000000000000000, 0.9510565162951535312, 1.000000000000000000, 0.9510565162951535312, 1.000000000000000000, 0.9510565162951535312, 1.000000000000000000, 0.9510565162951535312, 1.000000000000000000, 0.9510565162951535312, 1.000000000000000000, 0.9510565162951535312, 1.000000000000000000, 0.9510565162951535312, 1.000000000000000000, 0.9510565162951535312, 1.000000000000000000, 0.9510565162951535312, 1.000000000000000000, 0.9510565162951535312, 1.000000000000000000, 0.9510565162951535312, 1.000000000000000000, 0.9510565162951535312, 1.000000000000000000, 0.9510565162951535312, 1.000000000000000000, 0.9510565162951535312, 1.000000000000000000, 0.9510565162951535312, 1.000000000000000000, 0.9510565162951535312, 1.000000000000000000, 0.9510565162951535312, 1.000000000000000000, 0.9510565162951535312, 1.000000000000000000, 0.9510565162951535312, 1.000000000000000000, 0.9510565162951535312, 1.000000000000000000, 0.9510565162951535312, 1.000000000000000000, 0.9510565162951535312, 1.000000000000000000, 0.9510565162951535312, 1.000000000000000000, 0.9510565162951535312, 1.000000000000000000, 0.9510565162951535312, 1.000000000000000000, 0.9510565162951535312, 1.000000000000000000, 0.9510565162951535312, 1.000000000000000000, 0.9510565162951535312, 1.000000000000000000, 0.9510565162951535312, 1.000000000000000000, 0.9510565162951535312, 1.000000000000000000, 0.9510565162951535312, 1.000000000000000000, 0.9510565162951535312, 1.000000000000000000, 0.9510565162951535312, 1.000000000000000000, 0.9510565162951535312, 1.000000000000000000, 0.9510565162951535312, 1.000000000000000000, 0.9510565162951535312, 1.000000000000000000, 0.9510565162951535312, 1.000000000000000000, 0.9510565162951535312, 1.000000000000000000, 0.9510565162951535312, 1.000000000000000000, 0.9510565162951535312, 1.000000000000000000, 0.9510565162951535312, 1.000000000000000000, 0.9510565162951535312, 1.000000000000000000, 0.9510565162951535312, 1.000000000000000000, 0.9510565162951535312, 1.000000000000000000, 0.9510565162951535312, 1.000000000000000000, 0.9510565162951535312, 1.000000000000000000, 0.9510565162951535312, 1.000000000000000000, 0.9510565162951535312, 1.000000000000000000, 0.9510565162951535312, 1.000000000000000000, 0.9510565162951535312, 1.000000000000000000, 0.9510565162951535312, 1.000000000000000000),
 ( 0.3333333333333333703, 0.3170188387650512141, 0.3333333333333333703, 0.3170188387650512141, 0.3333333333333333703, 0.3170188387650512141, 0.3333333333333333703, 0.3170188387650512141, 0.3333333333333333703, 0.3170188387650512141, 0.3333333333333333703, 0.3170188387650512141, 0.3333333333333333703, 0.3170188387650512141, 0.3333333333333333703, 0.3170188387650512141, 0.3333333333333333703, 0.3170188387650512141, 0.3333333333333333703, 0.3170188387650512141, 0.3333333333333333703, 0.3170188387650512141, 0.3333333333333333703, 0.3170188387650512141, 0.3333333333333333703, 0.3170188387650512141, 0.3333333333333333703, 0.3170188387650512141, 0.3333333333333333703, 0.3170188387650512141, 0.3333333333333333703, 0.3170188387650512141, 0.3333333333333333703, 0.3170188387650512141, 0.3333333333333333703, 0.3170188387650512141, 0.3333333333333333703, 0.3170188387650512141, 0.3333333333333333703, 0.3170188387650512141, 0.3333333333333333703, 0.3170188387650512141, 0.3333333333333333703, 0.3170188387650512141, 0.3333333333333333703, 0.3170188387650512141, 0.3333333333333333703, 0.3170188387650512141, 0.3333333333333333703, 0.3170188387650512141, 0.3333333333333333703, 0.3170188387650512141, 0.3333333333333333703, 0.3170188387650512141, 0.3333333333333333703, 0.3170188387650512141, 0.3333333333333333703, 0.3170188387650512141, 0.3333333333333333703, 0.3170188387650512141, 0.3333333333333333703, 0.3170188387650512141, 0.3333333333333333703, 0.3170188387650512141, 0.3333333333333333703, 0.3170188387650512141, 0.3333333333333333703, 0.3170188387650512141, 0.3333333333333333703, 0.3170188387650512141, 0.3333333333333333703, 0.3170188387650512141, 0.3333333333333333703, 0.3170188387650512141, 0.3333333333333333703, 0.3170188387650512141, 0.3333333333333333703, 0.3170188387650512141, 0.3333333333333333703, 0.3170188387650512141, 0.3333333333333333703, 0.3170188387650512141, 0.3333333333333333703, 0.3170188387650512141, 0.3333333333333333703, 0.3170188387650512141, 0.3333333333333333703, 0.3170188387650512141, 0.3333333333333333703, 0.3170188387650512141, 0.3333333333333333703, 0.3170188387650512141, 0.3333333333333333703, 0.3170188387650512141, 0.3333333333333333703, 0.3170188387650512141, 0.3333333333333333703, 0.3170188387650512141, 0.3333333333333333703, 0.3170188387650512141, 0.3333333333333333703, 0.3170188387650512141, 0.3333333333333333703, 0.3170188387650512141, 0.3333333333333333703, 0.3170188387650512141, 0.3333333333333333703, 0.3170188387650512141, 0.3333333333333333703, 0.3170188387650512141, 0.3333333333333333703, 0.3170188387650512141, 0.3333333333333333703, 0.3170188387650512141, 0.3333333333333333703, 0.3170188387650512141, 0.3333333333333333703, 0.3170188387650512141, 0.3333333333333333703, 0.3170188387650512141, 0.3333333333333333703, 0.3170188387650512141, 0.3333333333333333703, 0.3170188387650512141, 0.3333333333333333703, 0.3170188387650512141, 0.3333333333333333703, 0.3170188387650512141, 0.3333333333333333703, 0.3170188387650512141, 0.3333333333333333703, 0.3170188387650512141, 0.3333333333333333703, 0.3170188387650512141, 0.3333333333333333703, 0.3170188387650512141, 0.3333333333333333703, 0.3170188387650512141, 0.3333333333333333703, 0.3170188387650512141, 0.3333333333333333703),
 ( 0.3333333333333333703, 0.3170188387650512141, 0.3333333333333333703, 0.3170188387650512141, 0.3333333333333333703, 0.3170188387650512141, 0.3333333333333333703, 0.3170188387650512141, 0.3333333333333333703, 0.3170188387650512141, 0.3333333333333333703, 0.3170188387650512141, 0.3333333333333333703, 0.3170188387650512141, 0.3333333333333333703, 0.3170188387650512141, 0.3333333333333333703, 0.3170188387650512141, 0.3333333333333333703, 0.3170188387650512141, 0.3333333333333333703, 0.3170188387650512141, 0.3333333333333333703, 0.3170188387650512141, 0.3333333333333333703, 0.3170188387650512141, 0.3333333333333333703, 0.3170188387650512141, 0.3333333333333333703, 0.3170188387650512141, 0.3333333333333333703, 0.3170188387650512141, 0.3333333333333333703, 0.3170188387650512141, 0.3333333333333333703, 0.3170188387650512141, 0.3333333333333333703, 0.3170188387650512141, 0.3333333333333333703, 0.3170188387650512141, 0.3333333333333333703, 0.3170188387650512141, 0.3333333333333333703, 0.3170188387650512141, 0.3333333333333333703, 0.3170188387650512141, 0.3333333333333333703, 0.3170188387650512141, 0.3333333333333333703, 0.3170188387650512141, 0.3333333333333333703, 0.3170188387650512141, 0.3333333333333333703, 0.3170188387650512141, 0.3333333333333333703, 0.3170188387650512141, 0.3333333333333333703, 0.3170188387650512141, 0.3333333333333333703, 0.3170188387650512141, 0.3333333333333333703, 0.3170188387650512141, 0.3333333333333333703, 0.3170188387650512141, 0.3333333333333333703, 0.3170188387650512141, 0.3333333333333333703, 0.3170188387650512141, 0.3333333333333333703, 0.3170188387650512141, 0.3333333333333333703, 0.3170188387650512141, 0.3333333333333333703, 0.3170188387650512141, 0.3333333333333333703, 0.3170188387650512141, 0.3333333333333333703, 0.3170188387650512141, 0.3333333333333333703, 0.3170188387650512141, 0.3333333333333333703, 0.3170188387650512141, 0.3333333333333333703, 0.3170188387650512141, 0.3333333333333333703, 0.3170188387650512141, 0.3333333333333333703, 0.3170188387650512141, 0.3333333333333333703, 0.3170188387650512141, 0.3333333333333333703, 0.3170188387650512141, 0.3333333333333333703, 0.3170188387650512141, 0.3333333333333333703, 0.3170188387650512141, 0.3333333333333333703, 0.3170188387650512141, 0.3333333333333333703, 0.3170188387650512141, 0.3333333333333333703, 0.3170188387650512141, 0.3333333333333333703, 0.3170188387650512141, 0.3333333333333333703, 0.3170188387650512141, 0.3333333333333333703, 0.3170188387650512141, 0.3333333333333333703, 0.3170188387650512141, 0.3333333333333333703, 0.3170188387650512141, 0.3333333333333333703, 0.3170188387650512141, 0.3333333333333333703, 0.3170188387650512141, 0.3333333333333333703, 0.3170188387650512141, 0.3333333333333333703, 0.3170188387650512141, 0.3333333333333333703, 0.3170188387650512141, 0.3333333333333333703, 0.3170188387650512141, 0.3333333333333333703, 0.3170188387650512141, 0.3333333333333333703, 0.3170188387650512141, 0.3333333333333333703, 0.3170188387650512141, 0.3333333333333333703, 0.3170188387650512141, 0.3333333333333333703, 0.3170188387650512141, 0.3333333333333333703, 0.3170188387650512141, 0.3333333333333333703, 0.3170188387650512141, 0.3333333333333333703, 0.3170188387650512141, 0.3333333333333333703),
 ( 1.000000000000000000, 0.9510565162951535312, 1.000000000000000000, 0.9510565162951535312, 1.000000000000000000, 0.9510565162951535312, 1.000000000000000000, 0.9510565162951535312, 1.000000000000000000, 0.9510565162951535312, 1.000000000000000000, 0.9510565162951535312, 1.000000000000000000, 0.9510565162951535312, 1.000000000000000000, 0.9510565162951535312, 1.000000000000000000, 0.9510565162951535312, 1.000000000000000000, 0.9510565162951535312, 1.000000000000000000, 0.9510565162951535312, 1.000000000000000000, 0.9510565162951535312, 1.000000000000000000, 0.9510565162951535312, 1.000000000000000000, 0.9510565162951535312, 1.000000000000000000, 0.9510565162951535312, 1.000000000000000000, 0.9510565162951535312, 1.000000000000000000, 0.9510565162951535312, 1.000000000000000000, 0.9510565162951535312, 1.000000000000000000, 0.9510565162951535312, 1.000000000000000000, 0.9510565162951535312, 1.000000000000000000, 0.9510565162951535312, 1.000000000000000000, 0.9510565162951535312, 1.000000000000000000, 0.9510565162951535312, 1.000000000000000000, 0.9510565162951535312, 1.000000000000000000, 0.9510565162951535312, 1.000000000000000000, 0.9510565162951535312, 1.000000000000000000, 0.9510565162951535312, 1.000000000000000000, 0.9510565162951535312, 1.000000000000000000, 0.9510565162951535312, 1.000000000000000000, 0.9510565162951535312, 1.000000000000000000, 0.9510565162951535312, 1.000000000000000000, 0.9510565162951535312, 1.000000000000000000, 0.9510565162951535312, 1.000000000000000000, 0.9510565162951535312, 1.000000000000000000, 0.9510565162951535312, 1.000000000000000000, 0.9510565162951535312, 1.000000000000000000, 0.9510565162951535312, 1.000000000000000000, 0.9510565162951535312, 1.000000000000000000, 0.9510565162951535312, 1.000000000000000000, 0.9510565162951535312, 1.000000000000000000, 0.9510565162951535312, 1.000000000000000000, 0.9510565162951535312, 1.000000000000000000, 0.9510565162951535312, 1.000000000000000000, 0.9510565162951535312, 1.000000000000000000, 0.9510565162951535312, 1.000000000000000000, 0.9510565162951535312, 1.000000000000000000, 0.9510565162951535312, 1.000000000000000000, 0.9510565162951535312, 1.000000000000000000, 0.9510565162951535312, 1.000000000000000000, 0.9510565162951535312, 1.000000000000000000, 0.9510565162951535312, 1.000000000000000000, 0.9510565162951535312, 1.000000000000000000, 0.9510565162951535312, 1.000000000000000000, 0.9510565162951535312, 1.000000000000000000, 0.9510565162951535312, 1.000000000000000000, 0.9510565162951535312, 1.000000000000000000, 0.9510565162951535312, 1.000000000000000000, 0.9510565162951535312, 1.000000000000000000, 0.9510565162951535312, 1.000000000000000000, 0.9510565162951535312, 1.000000000000000000, 0.9510565162951535312, 1.000000000000000000, 0.9510565162951535312, 1.000000000000000000, 0.9510565162951535312, 1.000000000000000000, 0.9510565162951535312, 1.000000000000000000, 0.9510565162951535312, 1.000000000000000000, 0.9510565162951535312, 1.000000000000000000, 0.9510565162951535312, 1.000000000000000000, 0.9510565162951535312, 1.000000000000000000, 0.9510565162951535312, 1.000000000000000000, 0.9510565162951535312, 1.000000000000000000) ) ) 
 REPRESENTATION_ITEM ( '' )  SURFACE ( )  );
#5570 = EDGE_CURVE ( 'NONE', #8403, #8204, #7272, .T. ) ;
#5571 = ORIENTED_EDGE ( 'NONE', *, *, #7844, .T. ) ;
#5572 = CARTESIAN_POINT ( 'NONE',  ( 8.389419568037416259E-16, -49.56698729999997255, -95.84999999890753486 ) ) ;
#5573 = CARTESIAN_POINT ( 'NONE',  ( -3.535533905932736864, -41.46446609406723383, -99.90000000000000568 ) ) ;
#5574 = FACE_BOUND ( 'NONE', #7095, .T. ) ;
#5575 = CARTESIAN_POINT ( 'NONE',  ( -3.229347689422839451, -48.22934768942280925, -96.14999999890753202 ) ) ;
#5576 = CARTESIAN_POINT ( 'NONE',  ( -25.51052057033350096, -47.22506321083132974, 11.66673928690326179 ) ) ;
#5577 = FACE_BOUND ( 'NONE', #8468, .T. ) ;
#5578 = VERTEX_POINT ( 'NONE', #1376 ) ;
#5579 = AXIS2_PLACEMENT_3D ( 'NONE', #3637, #3551, #5824 ) ;
#5580 = EDGE_CURVE ( 'NONE', #2059, #5916, #947, .T. ) ;
#5581 = CARTESIAN_POINT ( 'NONE',  ( -31.38201786482021305, -40.29859572486944330, -8.387063443159975762 ) ) ;
#5582 = CARTESIAN_POINT ( 'NONE',  ( -37.06321265474346660, -44.25000000000000000, 7.063212654743582952 ) ) ;
#5583 = VERTEX_POINT ( 'NONE', #3329 ) ;
#5584 = CARTESIAN_POINT ( 'NONE',  ( -28.51387258211773812, -49.80000000000001137, 9.383039235653802379 ) ) ;
#5585 = FILL_AREA_STYLE ('',( #2120 ) ) ;
#5586 = CARTESIAN_POINT ( 'NONE',  ( -1.891708078845683039, -40.43301269999998482, -99.59999999890753486 ) ) ;
#5587 = CARTESIAN_POINT ( 'NONE',  ( 2.071067811865474173, -39.99999999999997158, -99.94999999781505551 ) ) ;
#5588 = EDGE_CURVE ( 'NONE', #8058, #1053, #3068, .T. ) ;
#5589 = CARTESIAN_POINT ( 'NONE',  ( 4.999999999999998224, -44.99999999999997158, -99.29999999781504982 ) ) ;
#5590 = AXIS2_PLACEMENT_3D ( 'NONE', #568, #3413, #3281 ) ;
#5591 = CARTESIAN_POINT ( 'NONE',  ( -1.891708078845683483, -49.56698729999997255, -99.09999999890753486 ) ) ;
#5592 = VERTEX_POINT ( 'NONE', #4734 ) ;
#5593 = AXIS2_PLACEMENT_3D ( 'NONE', #3573, #1622, #784 ) ;
#5594 = CARTESIAN_POINT ( 'NONE',  ( -24.02705286092866643, -45.50140427513058228, 6.047868141099968398 ) ) ;
#5595 = ADVANCED_FACE ( 'NONE', ( #10 ), #2000, .T. ) ;
#5596 = CIRCLE ( 'NONE', #2936, 1.000000000000000888 ) ;
#5597 = CARTESIAN_POINT ( 'NONE',  ( 9.184850993605145972E-16, -49.99999999999997158, -98.79300000002184845 ) ) ;
#5598 = CARTESIAN_POINT ( 'NONE',  ( -2.796473189345805913E-16, -40.43301269999997061, -95.44999999890752918 ) ) ;
#5599 = CARTESIAN_POINT ( 'NONE',  ( -36.01040764008574513, -48.00000000000000711, -6.010407640085605685 ) ) ;
#5600 = ADVANCED_FACE ( 'NONE', ( #5252 ), #2623, .F. ) ;
#5601 = DIRECTION ( 'NONE',  ( -0.000000000000000000, 0.000000000000000000, 1.000000000000000000 ) ) ;
#5602 = DIRECTION ( 'NONE',  ( -0.000000000000000000, 1.000000000000000000, -0.000000000000000000 ) ) ;
#5603 = CARTESIAN_POINT ( 'NONE',  ( -21.60464910494133406, -40.20000000000000995, 1.329692952841886155 ) ) ;
#5604 = CARTESIAN_POINT ( 'NONE',  ( -26.23123798130810158, -41.69806059905386064, 11.92074493419280756 ) ) ;
#5605 = DIRECTION ( 'NONE',  ( 0.000000000000000000, 0.000000000000000000, 1.000000000000000000 ) ) ;
#5606 = CARTESIAN_POINT ( 'NONE',  ( -34.53486167607238144, -30.15000000000000213, -8.900167166472096270 ) ) ;
#5607 = AXIS2_PLACEMENT_3D ( 'NONE', #6865, #4931, #5448 ) ;
#5608 = EDGE_CURVE ( 'NONE', #4084, #4999, #7707, .T. ) ;
#5609 = CARTESIAN_POINT ( 'NONE',  ( 2.518094901854496914, -40.63106805822869205, -100.0000000000000142 ) ) ;
#5610 = CARTESIAN_POINT ( 'NONE',  ( -34.31290974752564438, -38.10000000000000853, 8.464561979789547053 ) ) ;
#5611 = ORIENTED_EDGE ( 'NONE', *, *, #6484, .F. ) ;
#5612 = FACE_OUTER_BOUND ( 'NONE', #3745, .T. ) ;
#5613 = ADVANCED_FACE ( 'NONE', ( #8569 ), #3373, .T. ) ;
#5614 = VERTEX_POINT ( 'NONE', #7377 ) ;
#5615 = CARTESIAN_POINT ( 'NONE',  ( -21.59636165304264921, -35.19859572486944188, 1.277368040863740228 ) ) ;
#5616 = CARTESIAN_POINT ( 'NONE',  ( -38.92545601287626056, -45.84859572486944046, -4.485229520447501450 ) ) ;
#5617 = CARTESIAN_POINT ( 'NONE',  ( -31.27736804086391942, -29.30140427513058299, -8.403638346957361449 ) ) ;
#5618 = CARTESIAN_POINT ( 'NONE',  ( 4.566987300000000083, -46.89170807884564596, -97.29999999890752349 ) ) ;
#5619 = PRESENTATION_STYLE_ASSIGNMENT (( #1611 ) ) ;
#5620 = CARTESIAN_POINT ( 'NONE',  ( -34.48648245112668320, -42.76835092305881858, 11.66791272636412913 ) ) ;
#5621 = CARTESIAN_POINT ( 'NONE',  ( -3.229347689422840784, -41.77065231057713390, -98.74999999890751212 ) ) ;
#5622 = DIRECTION ( 'NONE',  ( 1.000000000000000000, 0.000000000000000000, 0.000000000000000000 ) ) ;
#5623 = CARTESIAN_POINT ( 'NONE',  ( -20.00000000000002487, 0.000000000000000000, -45.00000000000000000 ) ) ;
#5624 = B_SPLINE_CURVE_WITH_KNOTS ( 'NONE', 3,
 ( #6068, #3306, #8584, #6727, #7302, #6024, #4002, #1303, #548, #7393, #4709, #686, #3874, #3257, #5980, #2551, #7969, #8673 ),
 .UNSPECIFIED., .F., .F.,
 ( 4, 2, 2, 2, 2, 2, 2, 2, 4 ),
 ( 0.02369462427231871365, 0.02468136329545927640, 0.02566810231859983568, 0.02665484134174039843, 0.02764158036488095771, 0.02862831938802152046, 0.02961505841116208321, 0.03060179743430264249, 0.03158853645744319483 ),
 .UNSPECIFIED. ) ;
#5625 = CARTESIAN_POINT ( 'NONE',  ( 0.000000000000000000, -44.99999999999997158, -95.00000000000000000 ) ) ;
#5626 = ORIENTED_EDGE ( 'NONE', *, *, #1766, .T. ) ;
#5627 = CARTESIAN_POINT ( 'NONE',  ( -21.18131961722757595, -38.04859572486944330, -1.453139578080854699 ) ) ;
#5628 = CARTESIAN_POINT ( 'NONE',  ( -39.86591130483550671, -44.55000000000001137, 1.562606840307984468 ) ) ;
#5629 = VERTEX_POINT ( 'NONE', #1328 ) ;
#5630 = CARTESIAN_POINT ( 'NONE',  ( -28.38237549136062654, -29.45140427513057801, -9.857197362228843573 ) ) ;
#5631 = CIRCLE ( 'NONE', #6470, 12.00000000000000000 ) ;
#5632 =( NAMED_UNIT ( * ) PLANE_ANGLE_UNIT ( ) SI_UNIT ( $, .RADIAN. ) );
#5633 = LINE ( 'NONE', #8381, #1337 ) ;
#5634 = CARTESIAN_POINT ( 'NONE',  ( -2.071067811865475061, -39.99999999999997158, -100.6499999978150441 ) ) ;
#5635 = CARTESIAN_POINT ( 'NONE',  ( -26.64110105645932336, 8.000000000000000000, -25.00000000000000000 ) ) ;
#5636 = CARTESIAN_POINT ( 'NONE',  ( -1.891708078845683039, -40.43301269999998482, -96.99999999890752633 ) ) ;
#5637 = ORIENTED_EDGE ( 'NONE', *, *, #4868, .T. ) ;
#5638 = CARTESIAN_POINT ( 'NONE',  ( -22.03669253526174998, -34.35000000000000853, 4.057507815433014642 ) ) ;
#5639 = AXIS2_PLACEMENT_3D ( 'NONE', #38, #2742, #5410 ) ;
#5640 = CARTESIAN_POINT ( 'NONE',  ( 2.071067811865477282, -49.99999999999996447, -99.54300000002184845 ) ) ;
#5641 = UNCERTAINTY_MEASURE_WITH_UNIT (LENGTH_MEASURE( 1.000000000000000082E-05 ), #1028, 'distance_accuracy_value', 'NONE');
#5642 = FACE_OUTER_BOUND ( 'NONE', #646, .T. ) ;
#5643 = CARTESIAN_POINT ( 'NONE',  ( 9.184850993605145972E-16, -49.99999999999997158, -96.29999999781504982 ) ) ;
#5644 = DIRECTION ( 'NONE',  ( 0.000000000000000000, 0.000000000000000000, 1.000000000000000000 ) ) ;
#5645 = PRESENTATION_LAYER_ASSIGNMENT (  '', '', ( #5089 ) ) ;
#5646 = CARTESIAN_POINT ( 'NONE',  ( 3.535533905932737309, -48.53553390593270933, -100.1999999978150555 ) ) ;
#5647 = EDGE_CURVE ( 'NONE', #4635, #1100, #6048, .T. ) ;
#5648 = CARTESIAN_POINT ( 'NONE',  ( -25.94249218456686279, -37.65000000000000568, 7.963307464738195840 ) ) ;
#5649 = DIRECTION ( 'NONE',  ( 0.000000000000000000, 0.000000000000000000, 1.000000000000000000 ) ) ;
#5650 = AXIS2_PLACEMENT_3D ( 'NONE', #1949, #3233, #2 ) ;
#5651 = CARTESIAN_POINT ( 'NONE',  ( -26.64110105645932336, 8.000000000000000000, 124.0000000000000000 ) ) ;
#5652 = CARTESIAN_POINT ( 'NONE',  ( -31.48612741788231517, -36.30000000000000426, -9.383039235653804155 ) ) ;
#5653 = LINE ( 'NONE', #7506, #4233 ) ;
#5654 = CARTESIAN_POINT ( 'NONE',  ( -22.93678734525658314, -39.75000000000000000, -7.063212654743582064 ) ) ;
#5655 = ORIENTED_EDGE ( 'NONE', *, *, #3277, .T. ) ;
#5656 = CARTESIAN_POINT ( 'NONE',  ( -36.01040764008574513, -51.00000000000000711, -6.010407640085605685 ) ) ;
#5657 = ORIENTED_EDGE ( 'NONE', *, *, #7332, .F. ) ;
#5658 = CARTESIAN_POINT ( 'NONE',  ( -36.04786814110010340, -39.99859572486943904, -5.972947139071243861 ) ) ;
#5659 = CARTESIAN_POINT ( 'NONE',  ( -34.26570676250101855, -51.09859572486944046, 8.488613101951703044 ) ) ;
#5660 = CONICAL_SURFACE ( 'NONE', #6503, 2.099999999999997868, 1.029744258676652313 ) ;
#5661 = CARTESIAN_POINT ( 'NONE',  ( -38.38706344316003793, -31.70140427513057091, -1.382017864820032083 ) ) ;
#5662 = CARTESIAN_POINT ( 'NONE',  ( 4.566987299999998307, -44.99999999999997158, -98.04999999890752349 ) ) ;
#5663 = CARTESIAN_POINT ( 'NONE',  ( -2.796473189345805913E-16, -40.43301269999997061, -100.4499999989075292 ) ) ;
#5664 = CARTESIAN_POINT ( 'NONE',  ( -28.51387258211773812, -31.80000000000000782, 9.383039235653802379 ) ) ;
#5665 = CIRCLE ( 'NONE', #5239, 10.00000000000000178 ) ;
#5666 = CARTESIAN_POINT ( 'NONE',  ( -1.891708078845683483, -49.56698729999997255, -98.49999999890752633 ) ) ;
#5667 = EDGE_CURVE ( 'NONE', #3178, #4798, #1222, .T. ) ;
#5668 = CARTESIAN_POINT ( 'NONE',  ( -4.999999999999998224, -44.99999999999997158, -95.34999999890753486 ) ) ;
#5669 = CARTESIAN_POINT ( 'NONE',  ( 3.229347689422841228, -48.22934768942280925, -96.74999999890751212 ) ) ;
#5670 = ORIENTED_EDGE ( 'NONE', *, *, #834, .T. ) ;
#5671 = CARTESIAN_POINT ( 'NONE',  ( -26.18828373723858149, -37.59859572486943335, -7.597606577763319713 ) ) ;
#5672 = CARTESIAN_POINT ( 'NONE',  ( -34.53486167607238144, -42.15000000000001279, -8.900167166472096270 ) ) ;
#5673 = CIRCLE ( 'NONE', #7082, 4.999999999999969802 ) ;
#5674 = ORIENTED_EDGE ( 'NONE', *, *, #6794, .T. ) ;
#5675 = CARTESIAN_POINT ( 'NONE',  ( -23.31994607974211675, -30.50140427513058583, 6.754974922286503869 ) ) ;
#5676 = DIRECTION ( 'NONE',  ( -0.000000000000000000, -0.000000000000000000, 1.000000000000000000 ) ) ;
#5677 = CARTESIAN_POINT ( 'NONE',  ( 4.999999999999998224, -44.99999999999997158, -96.20000000000000284 ) ) ;
#5678 = CARTESIAN_POINT ( 'NONE',  ( -2.071067811865475061, -39.99999999999997158, -98.24999999781506688 ) ) ;
#5679 = DIRECTION ( 'NONE',  ( -0.000000000000000000, -0.000000000000000000, -1.000000000000000000 ) ) ;
#5680 = CARTESIAN_POINT ( 'NONE',  ( -2.071067811865475505, -49.99999999999996447, -97.25000000000000000 ) ) ;
#5681 = VERTEX_POINT ( 'NONE', #3897 ) ;
#5682 = MECHANICAL_DESIGN_GEOMETRIC_PRESENTATION_REPRESENTATION (  '', ( #3846 ), #7224 ) ;
#5683 = CARTESIAN_POINT ( 'NONE',  ( -21.60464910494133406, -34.20000000000000995, 1.329692952841886155 ) ) ;
#5684 = PRODUCT_DEFINITION_SHAPE ( 'NONE', 'NONE',  #8726 ) ;
#5685 = EDGE_CURVE ( 'NONE', #1617, #3140, #6575, .T. ) ;
#5686 = ORIENTED_EDGE ( 'NONE', *, *, #7019, .T. ) ;
#5687 = CARTESIAN_POINT ( 'NONE',  ( -4.566987299999997418, -46.89170807884566727, -95.99999999890752633 ) ) ;
#5688 = CARTESIAN_POINT ( 'NONE',  ( -4.999999999999997335, -47.07106781186546129, -97.24999999781506688 ) ) ;
#5689 = DIRECTION ( 'NONE',  ( 0.000000000000000000, 0.000000000000000000, 1.000000000000000000 ) ) ;
#5690 = DIRECTION ( 'NONE',  ( -1.000000000000000000, 0.000000000000000000, 0.000000000000000000 ) ) ;
#5691 = EDGE_CURVE ( 'NONE', #999, #1072, #4601, .T. ) ;
#5692 = ADVANCED_FACE ( 'NONE', ( #3940 ), #376, .F. ) ;
#5693 = CARTESIAN_POINT ( 'NONE',  ( -37.57355545560112375, -41.40000000000000568, 3.858919247786223305 ) ) ;
#5694 = DIRECTION ( 'NONE',  ( 0.000000000000000000, 0.000000000000000000, 1.000000000000000000 ) ) ;
#5695 = CARTESIAN_POINT ( 'NONE',  ( -23.68028341417693738, -30.75000000000000000, -6.319716585823200283 ) ) ;
#5696 = CARTESIAN_POINT ( 'NONE',  ( -22.93678734525658314, -36.75000000000000711, -7.063212654743582952 ) ) ;
#5697 = DIRECTION ( 'NONE',  ( 0.000000000000000000, -1.000000000000000000, 8.560894001270036306E-16 ) ) ;
#5698 = CARTESIAN_POINT ( 'NONE',  ( -36.71751442127229836, -39.00000000000000711, -6.717514421272142044 ) ) ;
#5699 = VERTEX_POINT ( 'NONE', #3935 ) ;
#5700 = ORIENTED_EDGE ( 'NONE', *, *, #2998, .T. ) ;
#5701 = CARTESIAN_POINT ( 'NONE',  ( -23.71967171589458445, -37.74859572486943904, -6.359104887540838469 ) ) ;
#5702 = CARTESIAN_POINT ( 'NONE',  ( -31.48612741788231517, -30.30000000000000782, -9.383039235653804155 ) ) ;
#5703 = CARTESIAN_POINT ( 'NONE',  ( -21.51138689804841420, -47.90140427513058086, -4.265706762501151772 ) ) ;
#5704 = ADVANCED_FACE ( 'NONE', ( #6658 ), #8277, .T. ) ;
#5705 = CARTESIAN_POINT ( 'NONE',  ( -2.796473189345805913E-16, -40.43301269999997061, -98.64999999890753202 ) ) ;
#5706 = UNCERTAINTY_MEASURE_WITH_UNIT (LENGTH_MEASURE( 1.000000000000000082E-05 ), #3423, 'distance_accuracy_value', 'NONE');
#5707 = CARTESIAN_POINT ( 'NONE',  ( -30.00000000000002842, 0.000000000000000000, -26.00000000000000355 ) ) ;
#5708 = CARTESIAN_POINT ( 'NONE',  ( -39.38303923565386100, -32.70000000000000995, -1.486127417882099788 ) ) ;
#5709 = PRODUCT_DEFINITION_SHAPE ( 'NONE', 'NONE',  #2881 ) ;
#5710 = CARTESIAN_POINT ( 'NONE',  ( 4.566987299999998307, -43.10829192115428299, -99.79999999890752349 ) ) ;
#5711 = DIRECTION ( 'NONE',  ( -0.000000000000000000, -0.000000000000000000, 1.000000000000000000 ) ) ;
#5712 = AXIS2_PLACEMENT_3D ( 'NONE', #5273, #3756, #5694 ) ;
#5713 = CARTESIAN_POINT ( 'NONE',  ( 3.229347689422839895, -41.77065231057713390, -96.54999999890752349 ) ) ;
#5714 = DIRECTION ( 'NONE',  ( 1.000000000000000000, 0.000000000000000000, 0.000000000000000000 ) ) ;
#5715 = VERTEX_POINT ( 'NONE', #4729 ) ;
#5716 = CARTESIAN_POINT ( 'NONE',  ( -36.28032828410546529, -42.24859572486943904, 6.359104887540839357 ) ) ;
#5717 = CARTESIAN_POINT ( 'NONE',  ( -25.68709025247441602, -42.60000000000000853, -8.464561979789547053 ) ) ;
#5718 = ORIENTED_EDGE ( 'NONE', *, *, #441, .F. ) ;
#5719 = CARTESIAN_POINT ( 'NONE',  ( -38.48861310195163554, -31.40140427513058086, 4.265706762501153548 ) ) ;
#5720 = DIRECTION ( 'NONE',  ( -0.000000000000000000, 0.000000000000000000, 1.000000000000000000 ) ) ;
#5721 = CARTESIAN_POINT ( 'NONE',  ( 4.566987299999998307, -44.99999999999997158, -99.84999999890752065 ) ) ;
#5722 = CARTESIAN_POINT ( 'NONE',  ( 4.999999999999998224, -44.99999999999997158, -95.40000000000000568 ) ) ;
#5723 = AXIS2_PLACEMENT_3D ( 'NONE', #1383, #2008, #5386 ) ;
#5724 = CYLINDRICAL_SURFACE ( 'NONE', #6784, 11.99999999999983302 ) ;
#5725 = CARTESIAN_POINT ( 'NONE',  ( 3.535533905932737309, -48.53553390593270933, -96.29999999999999716 ) ) ;
#5726 = ORIENTED_EDGE ( 'NONE', *, *, #3403, .F. ) ;
#5727 = VECTOR ( 'NONE', #6450, 1000.000000000000000 ) ;
#5728 = CARTESIAN_POINT ( 'NONE',  ( -25.99212434019154472, -48.65140427513057375, 7.988596311142242890 ) ) ;
#5729 = COLOUR_RGB ( '', 0.08235294, 0.09019608, 0.10196078) ;
#5730 = ORIENTED_EDGE ( 'NONE', *, *, #7035, .T. ) ;
#5731 = ADVANCED_FACE ( 'NONE', ( #3979, #7458, #2618, #6043, #1416, #4112, #8653 ), #7414, .F. ) ;
#5732 = CARTESIAN_POINT ( 'NONE',  ( 5.000000000000000000, -47.07106781186545419, -98.65000000000000568 ) ) ;
#5733 = CARTESIAN_POINT ( 'NONE',  ( -4.999999999999998224, -42.92893218813448897, -97.34999999781506119 ) ) ;
#5734 = CYLINDRICAL_SURFACE ( 'NONE', #4805, 2.099999999999997868 ) ;
#5735 = ITEM_DEFINED_TRANSFORMATION ( 'NONE', 'NONE', #3133,  #2554 ) ;
#5736 = DIRECTION ( 'NONE',  ( -0.000000000000000000, -0.000000000000000000, 1.000000000000000000 ) ) ;
#5737 = AXIS2_PLACEMENT_3D ( 'NONE', #8479, #1782, #7682 ) ;
#5738 = CARTESIAN_POINT ( 'NONE',  ( -22.03669253526174998, -43.35000000000000853, 4.057507815433014642 ) ) ;
#5739 = PLANE ( 'NONE',  #4763 ) ;
#5740 = LINE ( 'NONE', #4624, #481 ) ;
#5741 = DIRECTION ( 'NONE',  ( 0.000000000000000000, 0.000000000000000000, -1.000000000000000000 ) ) ;
#5742 = CARTESIAN_POINT ( 'NONE',  ( -25.46513832392765408, -34.64999999999998437, 8.900167166472096270 ) ) ;
#5743 = ADVANCED_FACE ( 'NONE', ( #1951 ), #1372, .F. ) ;
#5744 = FACE_OUTER_BOUND ( 'NONE', #2348, .T. ) ;
#5745 = CARTESIAN_POINT ( 'NONE',  ( -31.56260684030781505, -37.94999999999999574, 9.865911304835508489 ) ) ;
#5746 = VERTEX_POINT ( 'NONE', #4636 ) ;
#5747 = CARTESIAN_POINT ( 'NONE',  ( -34.58449383169706692, -31.14859572486944828, -8.874878320068054549 ) ) ;
#5748 = CARTESIAN_POINT ( 'NONE',  ( -28.46154767013959486, -50.79859572486945041, 9.374751783755112200 ) ) ;
#5749 = CARTESIAN_POINT ( 'NONE',  ( -21.61293655684001536, -30.20140427513057446, 1.382017864820032971 ) ) ;
#5750 = CARTESIAN_POINT ( 'NONE',  ( -4.566987299999998307, -44.99999999999997158, -98.44999999890752918 ) ) ;
#5751 = CARTESIAN_POINT ( 'NONE',  ( 30.32909313480922009, -40.00809359540121335, 12.49675575313100850 ) ) ;
#5752 = CARTESIAN_POINT ( 'NONE',  ( -39.86591130483550671, -41.55000000000001137, 1.562606840307984468 ) ) ;
#5753 = FACE_OUTER_BOUND ( 'NONE', #1867, .T. ) ;
#5754 = FACE_OUTER_BOUND ( 'NONE', #4164, .T. ) ;
#5755 = CARTESIAN_POINT ( 'NONE',  ( 3.229347689422841228, -48.22934768942280925, -98.34999999890752065 ) ) ;
#5756 = EDGE_CURVE ( 'NONE', #1195, #3779, #2041, .T. ) ;
#5757 = DIRECTION ( 'NONE',  ( 0.000000000000000000, 0.000000000000000000, -1.000000000000000000 ) ) ;
#5758 = ORIENTED_EDGE ( 'NONE', *, *, #3928, .T. ) ;
#5759 = CARTESIAN_POINT ( 'NONE',  ( -38.40363834695740053, -45.69859572486943478, -1.277368040863739118 ) ) ;
#5760 = CARTESIAN_POINT ( 'NONE',  ( -20.13408869516453947, -46.05000000000001137, -1.562606840307983136 ) ) ;
#5761 = EDGE_CURVE ( 'NONE', #8500, #7164, #8035, .T. ) ;
#5762 = EDGE_LOOP ( 'NONE', ( #1526, #3218, #6301, #2344 ) ) ;
#5763 = CARTESIAN_POINT ( 'NONE',  ( -28.38237549136062654, -35.45140427513057801, -9.857197362228843573 ) ) ;
#5764 = CYLINDRICAL_SURFACE ( 'NONE', #6303, 4.999999999999998224 ) ;
#5765 = DIRECTION ( 'NONE',  ( 0.000000000000000000, -1.000000000000000000, 0.000000000000000000 ) ) ;
#5766 = CARTESIAN_POINT ( 'NONE',  ( 12.65000000000000036, 1.549178200921401754E-15, 0.000000000000000000 ) ) ;
#5767 = CARTESIAN_POINT ( 'NONE',  ( -30.00000000000002487, 0.000000000000000000, -29.65000000000000213 ) ) ;
#5768 = CARTESIAN_POINT ( 'NONE',  ( 4.999999999999998224, -42.92893218813448897, -95.34999999999999432 ) ) ;
#5769 = ORIENTED_EDGE ( 'NONE', *, *, #2621, .F. ) ;
#5770 = APPLICATION_CONTEXT ( 'automotive_design' ) ;
#5771 = CARTESIAN_POINT ( 'NONE',  ( -23.68028341417693738, -30.75000000000000000, -6.319716585823198507 ) ) ;
#5772 = CIRCLE ( 'NONE', #8319, 2.099999999999997868 ) ;
#5773 = ORIENTED_EDGE ( 'NONE', *, *, #4060, .T. ) ;
#5774 = CARTESIAN_POINT ( 'NONE',  ( 2.071067811865477282, -49.99999999999996447, -96.35000000000000853 ) ) ;
#5775 = EDGE_CURVE ( 'NONE', #1907, #5205, #6155, .T. ) ;
#5776 = CARTESIAN_POINT ( 'NONE',  ( -3.061616997868382155E-16, -39.99999999999997158, -95.89999999781505835 ) ) ;
#5777 = VECTOR ( 'NONE', #2801, 1000.000000000000000 ) ;
#5778 = CARTESIAN_POINT ( 'NONE',  ( 34.99999999999998579, -44.99999999999995737, 11.45643923738957071 ) ) ;
#5779 = DIRECTION ( 'NONE',  ( 0.000000000000000000, 0.000000000000000000, 1.000000000000000000 ) ) ;
#5780 = AXIS2_PLACEMENT_3D ( 'NONE', #1545, #2311, #4283 ) ;
#5781 = CARTESIAN_POINT ( 'NONE',  ( -3.535533905932736864, -41.46446609406723383, -99.79999999781504982 ) ) ;
#5782 = CARTESIAN_POINT ( 'NONE',  ( -41.99999999999996447, 60.00000000000002842, 22.00000000000000000 ) ) ;
#5783 = FACE_OUTER_BOUND ( 'NONE', #2723, .T. ) ;
#5784 = DIRECTION ( 'NONE',  ( 0.000000000000000000, 0.5150380749100563760, 0.8571673007021110013 ) ) ;
#5785 = CARTESIAN_POINT ( 'NONE',  ( -37.06321265474346660, -38.25000000000000711, 7.063212654743582952 ) ) ;
#5786 =( NAMED_UNIT ( * ) SI_UNIT ( $, .STERADIAN. ) SOLID_ANGLE_UNIT ( ) );
#5787 = ORIENTED_EDGE ( 'NONE', *, *, #629, .T. ) ;
#5788 = CARTESIAN_POINT ( 'NONE',  ( -25.73429323749904185, -31.59859572486943335, -8.488613101951701267 ) ) ;
#5789 = CARTESIAN_POINT ( 'NONE',  ( -31.56260684030781505, -40.95000000000000995, 9.865911304835510265 ) ) ;
#5790 = CARTESIAN_POINT ( 'NONE',  ( -33.90612223281073057, -37.10140427513057659, 7.549504333439023718 ) ) ;
#5791 =( GEOMETRIC_REPRESENTATION_CONTEXT ( 3 ) GLOBAL_UNCERTAINTY_ASSIGNED_CONTEXT ( ( #7028 ) ) GLOBAL_UNIT_ASSIGNED_CONTEXT ( ( #6053, #2005, #6714 ) ) REPRESENTATION_CONTEXT ( 'NONE', 'WORKASPACE' ) );
#5792 = ADVANCED_FACE ( 'NONE', ( #3458 ), #6090, .F. ) ;
#5793 = UNCERTAINTY_MEASURE_WITH_UNIT (LENGTH_MEASURE( 1.000000000000000082E-05 ), #590, 'distance_accuracy_value', 'NONE');
#5794 = DIRECTION ( 'NONE',  ( 1.000000000000000000, 0.000000000000000000, 0.000000000000000000 ) ) ;
#5795 = CARTESIAN_POINT ( 'NONE',  ( -22.93678734525658314, -36.75000000000000711, -7.063212654743582952 ) ) ;
#5796 = DIRECTION ( 'NONE',  ( -0.000000000000000000, -0.000000000000000000, 1.000000000000000000 ) ) ;
#5797 = DIRECTION ( 'NONE',  ( 0.000000000000000000, -1.000000000000000000, -0.000000000000000000 ) ) ;
#5798 = CARTESIAN_POINT ( 'NONE',  ( 4.566987299999998307, -44.99999999999997158, -97.44999999890751496 ) ) ;
#5799 = PLANE ( 'NONE',  #5082 ) ;
#5800 = ORIENTED_EDGE ( 'NONE', *, *, #8511, .T. ) ;
#5801 = DIRECTION ( 'NONE',  ( 0.000000000000000000, 0.000000000000000000, 1.000000000000000000 ) ) ;
#5802 = AXIS2_PLACEMENT_3D ( 'NONE', #2616, #1237, #6569 ) ;
#5803 = CARTESIAN_POINT ( 'NONE',  ( -28.46154767013959486, -32.79859572486943620, 9.374751783755112200 ) ) ;
#5804 = CARTESIAN_POINT ( 'NONE',  ( -23.28248557872775137, -49.50000000000000711, 6.717514421272141156 ) ) ;
#5805 = EDGE_LOOP ( 'NONE', ( #3823, #6205, #2007, #1136 ) ) ;
#5806 = AXIS2_PLACEMENT_3D ( 'NONE', #175, #1534, #6957 ) ;
#5807 = CARTESIAN_POINT ( 'NONE',  ( -38.48861310195163554, -40.40140427513058086, 4.265706762501153548 ) ) ;
#5809 = CYLINDRICAL_SURFACE ( 'NONE', #7006, 4.999999999999998224 ) ;
#5808 =( BOUNDED_SURFACE ( )  B_SPLINE_SURFACE ( 1, 2, ( 
 ( #6963, #3666, #7054, #2308, #5598, #6346, #8300, #928, #1497, #133, #3622, #7670, #1013, #309, #8216, #5687, #8389, #3709, #2350, #180, #2833, #4192, #6874, #2261, #836, #3539, #6217, #5552, #8258, #2219, #4902, #7581, #1542, #4237, #2788, #5636, #1492, #4807, #8336, #4983, #5548, #176, #3491, #2301, #5453, #875, #7665, #2169, #2213, #3534, #1626, #2828, #4147, #6869, #2124, #6299, #129, #6825, #789, #7532, #2919, #4319, #259, #5501, #2257, #3577, #7003, #4230, #6173, #8253, #6261, #6958, #965, #6212, #832, #1582, #2875, #5591, #2962, #8210, #4855, #4897, #217, #8296, #4935, #7575, #4189, #1535, #6125, #6913, #8164, #7617, #4275, #922, #7489, #81, #3618, #1454, #304, #2390, #2468 ),
 ( #4406, #7841, #7094, #420, #3830, #3703, #1674, #5768, #1096, #3135, #5151, #6428, #1006, #384, #3661, #8467, #3006, #1808, #8506, #2343, #3090, #1052, #7047, #7218, #7800, #2429, #5725, #2513, #5108, #1768, #4449, #3744, #4364, #8384, #5189, #3790, #4489, #343, #7133, #5813, #6384, #7885, #6467, #1135, #5065, #5680, #3051, #7174, #6509, #1850, #462, #8426, #3177, #5854, #8546, #4533, #6340, #5024, #7715, #7755, #1720, #6683, #1259, #1933, #8714, #5900, #2643, #7349, #7259, #2552, #4619, #4660, #3348, #4047, #4710, #5314, #28, #1181, #8015, #1304, #8633, #5939, #1972, #3258, #4003, #6636, #594, #7970, #6552, #687, #5269, #8585, #3393, #2729, #3307, #3958, #1220, #6069, #503, #641, #5399 ) ),
 .UNSPECIFIED., .F., .F., .T. ) 
 B_SPLINE_SURFACE_WITH_KNOTS ( ( 2, 2 ),
 ( 3, 2, 2, 2, 2, 2, 2, 2, 2, 2, 2, 2, 2, 2, 2, 2, 2, 2, 2, 2, 2, 2, 2, 2, 2, 2, 2, 2, 2, 2, 2, 2, 2, 2, 2, 2, 2, 2, 2, 2, 2, 2, 2, 2, 2, 2, 2, 2, 2, 2, 3 ),
 ( 0.000000000000000000, 1.000000000000000000 ),
 ( 0.000000000000000000, 0.01785714285714285615, 0.03571428571428571230, 0.05357142857142856845, 0.07142857142857142461, 0.08928571428571428770, 0.1071428571428571369, 0.1250000000000000000, 0.1428571428571428492, 0.1607142857142857262, 0.1785714285714285754, 0.1964285714285714246, 0.2142857142857142738, 0.2321428571428571508, 0.2500000000000000000, 0.2678571428571428492, 0.2857142857142856984, 0.3035714285714285476, 0.3214285714285714524, 0.3392857142857143016, 0.3571428571428571508, 0.3750000000000000000, 0.3928571428571428492, 0.4107142857142856984, 0.4285714285714285476, 0.4464285714285714524, 0.4642857142857143016, 0.4821428571428571508, 0.5000000000000000000, 0.5178571428571429047, 0.5357142857142856984, 0.5535714285714286031, 0.5714285714285713969, 0.5892857142857143016, 0.6071428571428570953, 0.6250000000000000000, 0.6428571428571429047, 0.6607142857142856984, 0.6785714285714286031, 0.6964285714285713969, 0.7142857142857143016, 0.7321428571428570953, 0.7500000000000000000, 0.7678571428571429047, 0.7857142857142856984, 0.8035714285714286031, 0.8214285714285713969, 0.8392857142857143016, 0.8571428571428570953, 0.8750000000000000000, 0.8928571428571429047 ),
 .UNSPECIFIED. ) 
 GEOMETRIC_REPRESENTATION_ITEM ( )  RATIONAL_B_SPLINE_SURFACE ( (
 ( 1.000000000000000000, 0.9238795325112867385, 1.000000000000000000, 0.9238795325112867385, 1.000000000000000000, 0.9238795325112867385, 1.000000000000000000, 0.9238795325112867385, 1.000000000000000000, 0.9238795325112867385, 1.000000000000000000, 0.9238795325112867385, 1.000000000000000000, 0.9238795325112867385, 1.000000000000000000, 0.9238795325112867385, 1.000000000000000000, 0.9238795325112867385, 1.000000000000000000, 0.9238795325112867385, 1.000000000000000000, 0.9238795325112867385, 1.000000000000000000, 0.9238795325112867385, 1.000000000000000000, 0.9238795325112867385, 1.000000000000000000, 0.9238795325112867385, 1.000000000000000000, 0.9238795325112867385, 1.000000000000000000, 0.9238795325112867385, 1.000000000000000000, 0.9238795325112867385, 1.000000000000000000, 0.9238795325112867385, 1.000000000000000000, 0.9238795325112867385, 1.000000000000000000, 0.9238795325112867385, 1.000000000000000000, 0.9238795325112867385, 1.000000000000000000, 0.9238795325112867385, 1.000000000000000000, 0.9238795325112867385, 1.000000000000000000, 0.9238795325112867385, 1.000000000000000000, 0.9238795325112867385, 1.000000000000000000, 0.9238795325112867385, 1.000000000000000000, 0.9238795325112867385, 1.000000000000000000, 0.9238795325112867385, 1.000000000000000000, 0.9238795325112867385, 1.000000000000000000, 0.9238795325112867385, 1.000000000000000000, 0.9238795325112867385, 1.000000000000000000, 0.9238795325112867385, 1.000000000000000000, 0.9238795325112867385, 1.000000000000000000, 0.9238795325112867385, 1.000000000000000000, 0.9238795325112867385, 1.000000000000000000, 0.9238795325112867385, 1.000000000000000000, 0.9238795325112867385, 1.000000000000000000, 0.9238795325112867385, 1.000000000000000000, 0.9238795325112867385, 1.000000000000000000, 0.9238795325112867385, 1.000000000000000000, 0.9238795325112867385, 1.000000000000000000, 0.9238795325112867385, 1.000000000000000000, 0.9238795325112867385, 1.000000000000000000, 0.9238795325112867385, 1.000000000000000000, 0.9238795325112867385, 1.000000000000000000, 0.9238795325112867385, 1.000000000000000000, 0.9238795325112867385, 1.000000000000000000, 0.9238795325112867385, 1.000000000000000000, 0.9238795325112867385, 1.000000000000000000, 0.9238795325112867385, 1.000000000000000000),
 ( 1.000000000000000000, 0.9238795325112867385, 1.000000000000000000, 0.9238795325112867385, 1.000000000000000000, 0.9238795325112867385, 1.000000000000000000, 0.9238795325112867385, 1.000000000000000000, 0.9238795325112867385, 1.000000000000000000, 0.9238795325112867385, 1.000000000000000000, 0.9238795325112867385, 1.000000000000000000, 0.9238795325112867385, 1.000000000000000000, 0.9238795325112867385, 1.000000000000000000, 0.9238795325112867385, 1.000000000000000000, 0.9238795325112867385, 1.000000000000000000, 0.9238795325112867385, 1.000000000000000000, 0.9238795325112867385, 1.000000000000000000, 0.9238795325112867385, 1.000000000000000000, 0.9238795325112867385, 1.000000000000000000, 0.9238795325112867385, 1.000000000000000000, 0.9238795325112867385, 1.000000000000000000, 0.9238795325112867385, 1.000000000000000000, 0.9238795325112867385, 1.000000000000000000, 0.9238795325112867385, 1.000000000000000000, 0.9238795325112867385, 1.000000000000000000, 0.9238795325112867385, 1.000000000000000000, 0.9238795325112867385, 1.000000000000000000, 0.9238795325112867385, 1.000000000000000000, 0.9238795325112867385, 1.000000000000000000, 0.9238795325112867385, 1.000000000000000000, 0.9238795325112867385, 1.000000000000000000, 0.9238795325112867385, 1.000000000000000000, 0.9238795325112867385, 1.000000000000000000, 0.9238795325112867385, 1.000000000000000000, 0.9238795325112867385, 1.000000000000000000, 0.9238795325112867385, 1.000000000000000000, 0.9238795325112867385, 1.000000000000000000, 0.9238795325112867385, 1.000000000000000000, 0.9238795325112867385, 1.000000000000000000, 0.9238795325112867385, 1.000000000000000000, 0.9238795325112867385, 1.000000000000000000, 0.9238795325112867385, 1.000000000000000000, 0.9238795325112867385, 1.000000000000000000, 0.9238795325112867385, 1.000000000000000000, 0.9238795325112867385, 1.000000000000000000, 0.9238795325112867385, 1.000000000000000000, 0.9238795325112867385, 1.000000000000000000, 0.9238795325112867385, 1.000000000000000000, 0.9238795325112867385, 1.000000000000000000, 0.9238795325112867385, 1.000000000000000000, 0.9238795325112867385, 1.000000000000000000, 0.9238795325112867385, 1.000000000000000000, 0.9238795325112867385, 1.000000000000000000, 0.9238795325112867385, 1.000000000000000000) ) ) 
 REPRESENTATION_ITEM ( '' )  SURFACE ( )  );
#5810 = CARTESIAN_POINT ( 'NONE',  ( 39.85000000000002274, -21.99999999999992184, 80.00000000000002842 ) ) ;
#5811 = CARTESIAN_POINT ( 'NONE',  ( 9.184850993605145972E-16, -49.99999999999997158, -97.19999999999998863 ) ) ;
#5812 = DIRECTION ( 'NONE',  ( -1.000000000000000000, -0.000000000000000000, -0.000000000000000000 ) ) ;
#5813 = CARTESIAN_POINT ( 'NONE',  ( 4.999999999999998224, -42.92893218813448897, -96.95000000000000284 ) ) ;
#5814 = ORIENTED_EDGE ( 'NONE', *, *, #6127, .T. ) ;
#5815 = CIRCLE ( 'NONE', #5375, 2.149999999999985256 ) ;
#5816 = CARTESIAN_POINT ( 'NONE',  ( -22.06198138166579170, -48.35140427513057659, 4.107139971057695682 ) ) ;
#5817 = AXIS2_PLACEMENT_3D ( 'NONE', #7344, #8710, #7966 ) ;
#5818 = ADVANCED_FACE ( 'NONE', ( #7324 ), #3326, .F. ) ;
#5819 = VERTEX_POINT ( 'NONE', #1324 ) ;
#5820 = PRODUCT_DEFINITION_CONTEXT ( 'detailed design', #6951, 'design' ) ;
#5821 = CARTESIAN_POINT ( 'NONE',  ( 4.999999999999998224, -44.99999999999997158, -97.79999999999999716 ) ) ;
#5822 = AXIS2_PLACEMENT_3D ( 'NONE', #59, #7336, #2053 ) ;
#5823 = CARTESIAN_POINT ( 'NONE',  ( 3.535533969928884801, -41.46446615806338087, -100.0000000000000142 ) ) ;
#5824 = DIRECTION ( 'NONE',  ( 0.000000000000000000, 0.000000000000000000, 1.000000000000000000 ) ) ;
#5825 = DIRECTION ( 'NONE',  ( 0.000000000000000000, 0.000000000000000000, 1.000000000000000000 ) ) ;
#5826 = DIRECTION ( 'NONE',  ( 0.000000000000000000, 0.000000000000000000, 1.000000000000000000 ) ) ;
#5827 = CARTESIAN_POINT ( 'NONE',  ( -4.999999999999998224, -44.99999999999997158, -97.29999999781504982 ) ) ;
#5828 = DIRECTION ( 'NONE',  ( -1.000000000000000000, 0.000000000000000000, 0.000000000000000000 ) ) ;
#5829 = CARTESIAN_POINT ( 'NONE',  ( -20.61696076434619584, -49.20000000000000995, 1.486127417882100676 ) ) ;
#5830 =( REPRESENTATION_RELATIONSHIP ('NONE','NONE', #2265, #3450 ) REPRESENTATION_RELATIONSHIP_WITH_TRANSFORMATION ( #1682 )SHAPE_REPRESENTATION_RELATIONSHIP( ) );
#5831 = EDGE_LOOP ( 'NONE', ( #8286, #7004, #7134, #1648 ) ) ;
#5832 = CARTESIAN_POINT ( 'NONE',  ( -22.97617564697422665, -31.74859572486943193, -7.102600956461224690 ) ) ;
#5833 = CARTESIAN_POINT ( 'NONE',  ( -36.71751442127229836, -33.00000000000000711, -6.717514421272142044 ) ) ;
#5834 = CARTESIAN_POINT ( 'NONE',  ( -36.35910488754074521, -40.25140427513058228, 6.280328284105565650 ) ) ;
#5835 = CARTESIAN_POINT ( 'NONE',  ( 3.229347689422839895, -41.77065231057713390, -98.74999999890752633 ) ) ;
#5836 = CARTESIAN_POINT ( 'NONE',  ( 33.97336238306395728, -41.94765302695299169, 11.85321826485148655 ) ) ;
#5837 = CARTESIAN_POINT ( 'NONE',  ( -20.60867331244750034, -35.19859572486944188, 1.433802505903951419 ) ) ;
#5838 = CARTESIAN_POINT ( 'NONE',  ( -28.51387258211773812, -37.80000000000000426, 9.383039235653802379 ) ) ;
#5839 = FACE_OUTER_BOUND ( 'NONE', #3566, .T. ) ;
#5840 = DIRECTION ( 'NONE',  ( -0.000000000000000000, -0.000000000000000000, 1.000000000000000000 ) ) ;
#5841 = CARTESIAN_POINT ( 'NONE',  ( -3.229347689422839451, -48.22934768942280925, -96.14999999890753202 ) ) ;
#5842 = DIRECTION ( 'NONE',  ( -1.000000000000000000, 0.000000000000000000, 0.000000000000000000 ) ) ;
#5843 = ORIENTED_EDGE ( 'NONE', *, *, #4849, .T. ) ;
#5844 = DIRECTION ( 'NONE',  ( 0.000000000000000000, 0.000000000000000000, 1.000000000000000000 ) ) ;
#5845 = CARTESIAN_POINT ( 'NONE',  ( -28.65689575858256077, -46.44859572486943478, -8.836108267985801845 ) ) ;
#5846 = CARTESIAN_POINT ( 'NONE',  ( -23.31994607974211675, -33.50140427513058228, 6.754974922286503869 ) ) ;
#5847 = ORIENTED_EDGE ( 'NONE', *, *, #5647, .T. ) ;
#5848 = ORIENTED_EDGE ( 'NONE', *, *, #7251, .F. ) ;
#5849 = CARTESIAN_POINT ( 'NONE',  ( -21.51138689804841420, -32.90140427513058086, -4.265706762501151772 ) ) ;
#5850 = CARTESIAN_POINT ( 'NONE',  ( 0.000000000000000000, -44.99999999999997158, -105.0000000000000142 ) ) ;
#5851 = DIRECTION ( 'NONE',  ( 0.000000000000000000, 0.000000000000000000, -1.000000000000000000 ) ) ;
#5852 = DIRECTION ( 'NONE',  ( -1.000000000000000000, 0.000000000000000000, 0.000000000000000000 ) ) ;
#5853 = CARTESIAN_POINT ( 'NONE',  ( -7.499999999999999112, -44.99999999999997158, -100.0000000000000000 ) ) ;
#5854 = CARTESIAN_POINT ( 'NONE',  ( 2.071067811865474173, -39.99999999999997158, -97.64999999999999147 ) ) ;
#5855 = ADVANCED_FACE ( 'NONE', ( #8691 ), #5420, .F. ) ;
#5856 = ORIENTED_EDGE ( 'NONE', *, *, #1157, .T. ) ;
#5857 = CARTESIAN_POINT ( 'NONE',  ( -22.03669253526174998, -43.35000000000000853, 4.057507815433014642 ) ) ;
#5858 = AXIS2_PLACEMENT_3D ( 'NONE', #70, #3523, #7479 ) ;
#5859 = CONICAL_SURFACE ( 'NONE', #7544, 2.099999999999997868, 1.029744258676652313 ) ;
#5860 = EDGE_CURVE ( 'NONE', #4874, #8058, #1995, .T. ) ;
#5861 = ORIENTED_EDGE ( 'NONE', *, *, #2103, .T. ) ;
#5862 = CARTESIAN_POINT ( 'NONE',  ( 2.071067811865477282, -49.99999999999996447, -97.95000000000000284 ) ) ;
#5863 = CARTESIAN_POINT ( 'NONE',  ( -1.135448125450190027, -40.09623321959037412, -100.0007921917414109 ) ) ;
#5864 = EDGE_CURVE ( 'NONE', #5143, #7654, #4008, .T. ) ;
#5865 = CARTESIAN_POINT ( 'NONE',  ( -22.40239342223677355, -35.90140427513058086, -3.811716262761597473 ) ) ;
#5866 = FACE_OUTER_BOUND ( 'NONE', #6596, .T. ) ;
#5867 = CARTESIAN_POINT ( 'NONE',  ( -24.64110105645932336, 8.000000000000000000, -24.00000000000000000 ) ) ;
#5868 = CARTESIAN_POINT ( 'NONE',  ( -28.60187809025093841, -39.45000000000000284, -8.827394325379140483 ) ) ;
#5869 = AXIS2_PLACEMENT_3D ( 'NONE', #162, #2905, #5534 ) ;
#5870 = CARTESIAN_POINT ( 'NONE',  ( 42.00000000000000711, 48.00000000000002842, 20.34999999999992326 ) ) ;
#5871 = CARTESIAN_POINT ( 'NONE',  ( -50.00000000000002842, 30.00000000000000000, 80.00000000000002842 ) ) ;
#5872 = AXIS2_PLACEMENT_3D ( 'NONE', #3199, #7998, #668 ) ;
#5873 = CARTESIAN_POINT ( 'NONE',  ( -50.00000000000002842, 0.000000000000000000, 0.000000000000000000 ) ) ;
#5874 = PRODUCT_DEFINITION ( 'UNKNOWN', '', #7062, #2218 ) ;
#5875 = VERTEX_POINT ( 'NONE', #6613 ) ;
#5876 = CARTESIAN_POINT ( 'NONE',  ( -36.28032828410546529, -48.24859572486943904, 6.359104887540839357 ) ) ;
#5877 = CARTESIAN_POINT ( 'NONE',  ( -28.43739315969223824, -39.45000000000000995, -9.865911304835512041 ) ) ;
#5878 = CARTESIAN_POINT ( 'NONE',  ( -24.02705286092866643, -39.50140427513058228, 6.047868141099968398 ) ) ;
#5879 = ADVANCED_FACE ( 'NONE', ( #5464 ), #2839, .T. ) ;
#5880 = CARTESIAN_POINT ( 'NONE',  ( 8.389419568037416259E-16, -49.56698729999997255, -99.84999999890753486 ) ) ;
#5881 = CIRCLE ( 'NONE', #3634, 2.000000000000000888 ) ;
#5882 = DIRECTION ( 'NONE',  ( 0.000000000000000000, 0.000000000000000000, 1.000000000000000000 ) ) ;
#5883 = CARTESIAN_POINT ( 'NONE',  ( -20.60867331244750034, -41.19859572486944188, 1.433802505903951419 ) ) ;
#5884 = CARTESIAN_POINT ( 'NONE',  ( -20.61696076434619584, -40.20000000000000995, 1.486127417882100676 ) ) ;
#5885 = CARTESIAN_POINT ( 'NONE',  ( -4.999999999999998224, -42.92893218813449607, -98.94999999781505551 ) ) ;
#5886 = EDGE_CURVE ( 'NONE', #2517, #120, #184, .T. ) ;
#5887 = CARTESIAN_POINT ( 'NONE',  ( -30.00000000000002487, 0.000000000000000000, -40.35000000000000142 ) ) ;
#5888 = CARTESIAN_POINT ( 'NONE',  ( -4.566987299999998307, -43.10829192115428299, -98.69999999890752918 ) ) ;
#5889 = PRODUCT_DEFINITION ( 'UNKNOWN', '', #3271, #5820 ) ;
#5890 = VERTEX_POINT ( 'NONE', #3017 ) ;
#5891 =( NAMED_UNIT ( * ) PLANE_ANGLE_UNIT ( ) SI_UNIT ( $, .RADIAN. ) );
#5892 = CARTESIAN_POINT ( 'NONE',  ( -34.58449383169706692, -34.14859572486943051, -8.874878320068054549 ) ) ;
#5893 = CARTESIAN_POINT ( 'NONE',  ( -36.71751442127229836, -51.00000000000000711, -6.717514421272142044 ) ) ;
#5894 = ORIENTED_EDGE ( 'NONE', *, *, #3769, .T. ) ;
#5895 = VERTEX_POINT ( 'NONE', #6351 ) ;
#5896 = CARTESIAN_POINT ( 'NONE',  ( -22.89739904353894318, -38.75140427513058228, -7.023824353025938549 ) ) ;
#5897 = CARTESIAN_POINT ( 'NONE',  ( -41.99999999999996447, 60.00000000000002842, -23.64999999999999858 ) ) ;
#5898 = CARTESIAN_POINT ( 'NONE',  ( -3.535533905932735532, -48.53553390593270933, -97.29999999999999716 ) ) ;
#5899 = CARTESIAN_POINT ( 'NONE',  ( -2.071067811865475505, -49.99999999999997158, -96.45000000000000284 ) ) ;
#5900 = CARTESIAN_POINT ( 'NONE',  ( -4.999999999999998224, -42.92893218813448897, -98.25000000000000000 ) ) ;
#5901 = ORIENTED_EDGE ( 'NONE', *, *, #428, .F. ) ;
#5902 = CARTESIAN_POINT ( 'NONE',  ( -21.60464910494133406, -43.20000000000000995, 1.329692952841886155 ) ) ;
#5903 = MANIFOLD_SOLID_BREP ( 'Sweep1', #2106 ) ;
#5904 = VERTEX_POINT ( 'NONE', #4947 ) ;
#5905 = DIRECTION ( 'NONE',  ( -0.000000000000000000, -0.000000000000000000, -1.000000000000000000 ) ) ;
#5906 = CARTESIAN_POINT ( 'NONE',  ( 3.535533905932736420, -41.46446609406723383, -96.10000000000000853 ) ) ;
#5907 = CARTESIAN_POINT ( 'NONE',  ( -20.13408869516453947, -31.05000000000000782, -1.562606840307983136 ) ) ;
#5908 = CARTESIAN_POINT ( 'NONE',  ( -2.944777139751900918, -49.07987410177226906, -100.0011278004036797 ) ) ;
#5909 = CARTESIAN_POINT ( 'NONE',  ( -37.93801861833426159, -31.85140427513056594, -4.107139971057695682 ) ) ;
#5910 =( BOUNDED_CURVE ( )  B_SPLINE_CURVE ( 2, ( #4726, #2222, #7497, #1459, #6040, #3410, #6876, #7410, #4771 ),
 .UNSPECIFIED., .F., .T. ) 
 B_SPLINE_CURVE_WITH_KNOTS ( ( 3, 2, 2, 2, 3 ),
 ( 0.000000000000000000, 0.01785714285714282840, 0.03571428571428565679, 0.05357142857142848519, 0.07142857142857131358 ),
 .UNSPECIFIED. ) 
 CURVE ( )  GEOMETRIC_REPRESENTATION_ITEM ( )  RATIONAL_B_SPLINE_CURVE ( ( 1.000000000000000000, 0.9238795325112867385, 1.000000000000000000, 0.9238795325112867385, 1.000000000000000000, 0.9238795325112867385, 1.000000000000000000, 0.9238795325112871826, 0.9999999999999995559 ) ) 
 REPRESENTATION_ITEM ( '' )  );
#5911 = CARTESIAN_POINT ( 'NONE',  ( 2.071067811865474173, -39.99999999999997158, -99.94999999781505551 ) ) ;
#5912 = CARTESIAN_POINT ( 'NONE',  ( -25.94249218456686279, -34.64999999999999858, 7.963307464738194952 ) ) ;
#5913 = CARTESIAN_POINT ( 'NONE',  ( -30.00000000000002487, 0.000000000000000000, -29.65000000000000213 ) ) ;
#5914 = DIRECTION ( 'NONE',  ( 1.000000000000000000, 0.000000000000000000, -0.000000000000000000 ) ) ;
#5915 =( NAMED_UNIT ( * ) SI_UNIT ( $, .STERADIAN. ) SOLID_ANGLE_UNIT ( ) );
#5916 = VERTEX_POINT ( 'NONE', #885 ) ;
#5917 = CARTESIAN_POINT ( 'NONE',  ( -33.81171626276147890, -45.09859572486944046, 7.597606577763319713 ) ) ;
#5918 = CARTESIAN_POINT ( 'NONE',  ( -34.53486167607238144, -33.15000000000001279, -8.900167166472096270 ) ) ;
#5919 = CARTESIAN_POINT ( 'NONE',  ( -37.93801861833426159, -37.85140427513057659, -4.107139971057695682 ) ) ;
#5920 = DIRECTION ( 'NONE',  ( -0.000000000000000000, 0.000000000000000000, 1.000000000000000000 ) ) ;
#5921 = CIRCLE ( 'NONE', #7471, 9.999999999999994671 ) ;
#5922 = CARTESIAN_POINT ( 'NONE',  ( 2.000000000000000000, 0.000000000000000000, 0.000000000000000000 ) ) ;
#5923 = CARTESIAN_POINT ( 'NONE',  ( -21.07454398712378918, -38.34859572486944046, 4.485229520447505003 ) ) ;
#5924 = CARTESIAN_POINT ( 'NONE',  ( -23.28248557872775137, -43.50000000000001421, 6.717514421272141156 ) ) ;
#5925 = CARTESIAN_POINT ( 'NONE',  ( -3.061616997868382155E-16, -39.99999999999997158, -99.09999999781504698 ) ) ;
#5926 = CARTESIAN_POINT ( 'NONE',  ( -50.00000000000002842, -30.00000000000000000, 80.00000000000002842 ) ) ;
#5927 = CARTESIAN_POINT ( 'NONE',  ( -4.566987299999998307, -44.99999999999997158, -98.64999999890751781 ) ) ;
#5928 = ORIENTED_EDGE ( 'NONE', *, *, #2305, .T. ) ;
#5929 = PRESENTATION_STYLE_ASSIGNMENT (( #7123 ) ) ;
#5930 = CARTESIAN_POINT ( 'NONE',  ( -21.59636165304264921, -50.19859572486944188, 1.277368040863740228 ) ) ;
#5931 = CARTESIAN_POINT ( 'NONE',  ( -31.43380250590416125, -35.30140427513057944, -9.391326687552492558 ) ) ;
#5932 = ORIENTED_EDGE ( 'NONE', *, *, #7811, .F. ) ;
#5933 = EDGE_LOOP ( 'NONE', ( #1920, #2235, #7802 ) ) ;
#5934 = CARTESIAN_POINT ( 'NONE',  ( -36.68005392025794009, -47.00140427513058938, -6.754974922286504757 ) ) ;
#5935 = DIRECTION ( 'NONE',  ( -0.000000000000000000, -0.000000000000000000, 1.000000000000000000 ) ) ;
#5936 = CARTESIAN_POINT ( 'NONE',  ( 2.071067811865474173, -39.99999999999997158, -99.25000000000000000 ) ) ;
#5937 = CARTESIAN_POINT ( 'NONE',  ( 9.184850993605145972E-16, -49.99999999999997158, -99.49999999781503845 ) ) ;
#5938 = DIRECTION ( 'NONE',  ( 0.000000000000000000, -0.5000000000000012212, -0.8660254037844380415 ) ) ;
#5939 = CARTESIAN_POINT ( 'NONE',  ( -4.999999999999998224, -42.92893218813448897, -99.05000000000001137 ) ) ;
#5940 = ORIENTED_EDGE ( 'NONE', *, *, #3384, .T. ) ;
#5941 = CARTESIAN_POINT ( 'NONE',  ( -23.68028341417693738, -39.74999999999999289, -6.319716585823198507 ) ) ;
#5942 = CIRCLE ( 'NONE', #4820, 2.000000000000001776 ) ;
#5943 = VECTOR ( 'NONE', #8018, 1000.000000000000000 ) ;
#5944 = CYLINDRICAL_SURFACE ( 'NONE', #2952, 9.999999999999994671 ) ;
#5945 = DIRECTION ( 'NONE',  ( -0.000000000000000000, -0.000000000000000000, 1.000000000000000000 ) ) ;
#5946 = CARTESIAN_POINT ( 'NONE',  ( 4.999999999999998224, -42.92893218813448897, -97.64999999781504414 ) ) ;
#5947 = CARTESIAN_POINT ( 'NONE',  ( -25.46513832392765408, -40.65000000000000568, 8.900167166472096270 ) ) ;
#5948 = CARTESIAN_POINT ( 'NONE',  ( 4.566987299999998307, -44.99999999999997158, -99.64999999890753202 ) ) ;
#5949 = AXIS2_PLACEMENT_3D ( 'NONE', #2245, #6945, #1394 ) ;
#5950 = CARTESIAN_POINT ( 'NONE',  ( -3.760469397705862526, -48.30756035107769719, -99.99941978915393292 ) ) ;
#5951 = CARTESIAN_POINT ( 'NONE',  ( -31.27736804086391942, -38.30140427513057944, -8.403638346957361449 ) ) ;
#5952 = VECTOR ( 'NONE', #5219, 1000.000000000000000 ) ;
#5953 = CARTESIAN_POINT ( 'NONE',  ( -4.999999999999998224, -42.92893218813448897, -97.44300000002183992 ) ) ;
#5954 = CARTESIAN_POINT ( 'NONE',  ( -21.60464910494133406, -40.20000000000000995, 1.329692952841886155 ) ) ;
#5955 = DIRECTION ( 'NONE',  ( -1.000000000000000000, 0.000000000000000000, 0.000000000000000000 ) ) ;
#5956 = CARTESIAN_POINT ( 'NONE',  ( -22.93678734525658314, -45.75000000000000000, -7.063212654743582064 ) ) ;
#5957 = ADVANCED_FACE ( 'NONE', ( #5512 ), #2295, .F. ) ;
#5958 = VERTEX_POINT ( 'NONE', #6179 ) ;
#5959 = DIRECTION ( 'NONE',  ( 0.000000000000000000, 0.000000000000000000, 1.000000000000000000 ) ) ;
#5960 = CARTESIAN_POINT ( 'NONE',  ( -39.38303923565386100, -32.70000000000000995, -1.486127417882099788 ) ) ;
#5961 = CARTESIAN_POINT ( 'NONE',  ( -38.83610826798580717, -46.55140427513058654, 1.343104241417631073 ) ) ;
#5962 = CIRCLE ( 'NONE', #6662, 2.099999999999997868 ) ;
#5963 = DIRECTION ( 'NONE',  ( -0.000000000000000000, 0.000000000000000000, 1.000000000000000000 ) ) ;
#5964 = DIRECTION ( 'NONE',  ( 1.000000000000000000, 0.000000000000000000, 0.000000000000000000 ) ) ;
#5965 = CARTESIAN_POINT ( 'NONE',  ( -39.85719736222883824, -33.54859572486944330, 1.617624508639602388 ) ) ;
#5966 = CARTESIAN_POINT ( 'NONE',  ( 3.535533905932736420, -41.46446609406723383, -99.19999999781505551 ) ) ;
#5967 = LINE ( 'NONE', #7870, #8375 ) ;
#5968 = CARTESIAN_POINT ( 'NONE',  ( -4.566987299999998307, -44.99999999999997158, -95.24999999890752633 ) ) ;
#5969 = EDGE_LOOP ( 'NONE', ( #8247, #8459, #5067 ) ) ;
#5970 = FACE_OUTER_BOUND ( 'NONE', #5805, .T. ) ;
#5971 = CARTESIAN_POINT ( 'NONE',  ( -34.05750781543318340, -45.14999999999999858, -7.963307464738195840 ) ) ;
#5972 = ADVANCED_FACE ( 'NONE', ( #2136 ), #8221, .T. ) ;
#5973 = CARTESIAN_POINT ( 'NONE',  ( -37.02382435302582309, -33.24859572486943193, 7.102600956461226467 ) ) ;
#5974 = CARTESIAN_POINT ( 'NONE',  ( -38.48861310195163554, -31.40140427513058086, 4.265706762501153548 ) ) ;
#5975 = EDGE_LOOP ( 'NONE', ( #2921, #6991, #3833, #816, #8184, #5626, #3947, #8034, #6959, #29, #8580, #6116, #421, #6730, #1825, #5565 ) ) ;
#5976 = CARTESIAN_POINT ( 'NONE',  ( -25.63988726744978663, -47.60140427513058370, -8.440510857627391061 ) ) ;
#5977 = DIRECTION ( 'NONE',  ( -0.000000000000000000, -0.000000000000000000, 1.000000000000000000 ) ) ;
#5978 = CARTESIAN_POINT ( 'NONE',  ( 2.000000000000000000, 0.8865213383406683745, -1.535500000000000753 ) ) ;
#5979 = CARTESIAN_POINT ( 'NONE',  ( 4.999999999999998224, -44.99999999999997158, -98.49999999781503845 ) ) ;
#5980 = CARTESIAN_POINT ( 'NONE',  ( 31.30777697610241006, -49.83705382567072917, 12.43557624291735841 ) ) ;
#5981 = DIRECTION ( 'NONE',  ( 1.000000000000000000, 0.000000000000000000, 0.000000000000000000 ) ) ;
#5982 = VERTEX_POINT ( 'NONE', #6966 ) ;
#5983 = CARTESIAN_POINT ( 'NONE',  ( -23.68028341417693738, -45.74999999999999289, -6.319716585823198507 ) ) ;
#5984 = PRODUCT_RELATED_PRODUCT_CATEGORY ( 'part', '', ( #1062 ) ) ;
#5985 = AXIS2_PLACEMENT_3D ( 'NONE', #4690, #2139, #6882 ) ;
#5986 = ORIENTED_EDGE ( 'NONE', *, *, #2951, .T. ) ;
#5987 = CARTESIAN_POINT ( 'NONE',  ( 1.891708078845682595, -40.43301269999998482, -98.89999999890751781 ) ) ;
#5988 = CARTESIAN_POINT ( 'NONE',  ( -4.999999999999998224, -42.92893218813448897, -95.74999999781503845 ) ) ;
#5989 = CARTESIAN_POINT ( 'NONE',  ( -21.09983283352784156, -46.34999999999998721, 4.534861676072186043 ) ) ;
#5990 = CARTESIAN_POINT ( 'NONE',  ( -3.229347689422839451, -48.22934768942280925, -99.94999999890752918 ) ) ;
#5991 = CARTESIAN_POINT ( 'NONE',  ( -33.35889894354067309, -7.999999999999996447, 124.0000000000000000 ) ) ;
#5992 = CARTESIAN_POINT ( 'NONE',  ( -34.00787565980851213, -38.15140427513058086, -7.988596311142238449 ) ) ;
#5993 = CARTESIAN_POINT ( 'NONE',  ( -4.999999999999998224, -44.99999999999997158, -94.99300000002185129 ) ) ;
#5994 = CARTESIAN_POINT ( 'NONE',  ( -34.05750781543319050, -33.15000000000000568, -7.963307464738194952 ) ) ;
#5995 = CARTESIAN_POINT ( 'NONE',  ( 29.33771720961957641, -49.96682304584948753, 12.48662461771946397 ) ) ;
#5996 = VECTOR ( 'NONE', #6804, 1000.000000000000000 ) ;
#5997 = CARTESIAN_POINT ( 'NONE',  ( -4.999999999999998224, -44.99999999999997158, -95.79999999999999716 ) ) ;
#5998 = CARTESIAN_POINT ( 'NONE',  ( 30.00000000000002842, 52.67500000000002558, 0.000000000000000000 ) ) ;
#5999 = ORIENTED_EDGE ( 'NONE', *, *, #2548, .F. ) ;
#6000 = DIRECTION ( 'NONE',  ( 1.000000000000000000, 0.000000000000000000, 0.000000000000000000 ) ) ;
#6001 = CARTESIAN_POINT ( 'NONE',  ( -31.48612741788231517, -45.30000000000000426, -9.383039235653804155 ) ) ;
#6002 = CARTESIAN_POINT ( 'NONE',  ( -21.61293655684001536, -48.20140427513058512, 1.382017864820032971 ) ) ;
#6003 = EDGE_CURVE ( 'NONE', #94, #6389, #7205, .T. ) ;
#6004 = CARTESIAN_POINT ( 'NONE',  ( 2.071067811865474173, -39.99999999999997158, -96.85000000000002274 ) ) ;
#6005 = CIRCLE ( 'NONE', #6707, 9.999999999999994671 ) ;
#6006 = DIRECTION ( 'NONE',  ( -0.000000000000000000, 1.000000000000000000, -0.000000000000000000 ) ) ;
#6007 = CARTESIAN_POINT ( 'NONE',  ( -38.44051085762733777, -36.39859572486944472, 4.360112732550414982 ) ) ;
#6008 = FACE_OUTER_BOUND ( 'NONE', #3704, .T. ) ;
#6009 = CYLINDRICAL_SURFACE ( 'NONE', #4556, 12.49999999999998046 ) ;
#6010 = CARTESIAN_POINT ( 'NONE',  ( 1.891708078845685481, -49.56698729999997255, -99.99999999890751212 ) ) ;
#6011 = AXIS2_PLACEMENT_3D ( 'NONE', #5850, #3086, #6336 ) ;
#6012 = PRESENTATION_STYLE_ASSIGNMENT (( #6670 ) ) ;
#6013 = ORIENTED_EDGE ( 'NONE', *, *, #6983, .F. ) ;
#6014 = CARTESIAN_POINT ( 'NONE',  ( -18.00000000000019185, 1.469576158976803042E-15, -41.35000000000000142 ) ) ;
#6015 = CARTESIAN_POINT ( 'NONE',  ( -38.82739432537914581, -50.55000000000001137, 1.398121909749243441 ) ) ;
#6016 = CARTESIAN_POINT ( 'NONE',  ( -20.60867331244750034, -41.19859572486944188, 1.433802505903951419 ) ) ;
#6017 = CARTESIAN_POINT ( 'NONE',  ( -22.89739904353894318, -44.75140427513058228, -7.023824353025938549 ) ) ;
#6018 = CIRCLE ( 'NONE', #2649, 1.000000000000000888 ) ;
#6019 = ORIENTED_EDGE ( 'NONE', *, *, #6970, .F. ) ;
#6020 = CARTESIAN_POINT ( 'NONE',  ( -28.56619749409589204, -48.80140427513057233, 9.391326687552490782 ) ) ;
#6021 = FACE_OUTER_BOUND ( 'NONE', #4385, .T. ) ;
#6022 = DIRECTION ( 'NONE',  ( -1.000000000000000000, -0.000000000000000000, -0.000000000000000000 ) ) ;
#6023 = CARTESIAN_POINT ( 'NONE',  ( 5.000000000000000000, -47.07106781186545419, -100.1499999978150441 ) ) ;
#6024 = CARTESIAN_POINT ( 'NONE',  ( 34.48947942966652391, -47.22506321083128711, 11.66673928690324225 ) ) ;
#6025 = LINE ( 'NONE', #4751, #1635 ) ;
#6026 = EDGE_LOOP ( 'NONE', ( #707, #3040, #2939 ) ) ;
#6027 = EDGE_CURVE ( 'NONE', #2692, #7413, #7996, .T. ) ;
#6028 = CARTESIAN_POINT ( 'NONE',  ( -37.57355545560112375, -44.40000000000000568, 3.858919247786223305 ) ) ;
#6029 = CARTESIAN_POINT ( 'NONE',  ( -38.90016716647221529, -35.84999999999998721, -4.534861676072185155 ) ) ;
#6030 = ORIENTED_EDGE ( 'NONE', *, *, #7814, .T. ) ;
#6031 = CARTESIAN_POINT ( 'NONE',  ( -3.229347689422839451, -48.22934768942280925, -99.34999999890752065 ) ) ;
#6032 = CARTESIAN_POINT ( 'NONE',  ( -4.999999999999998224, -44.99999999999997158, -99.79999999999999716 ) ) ;
#6033 = CARTESIAN_POINT ( 'NONE',  ( -31.56260684030781505, -40.95000000000000995, 9.865911304835510265 ) ) ;
#6034 = CARTESIAN_POINT ( 'NONE',  ( -1.891708078845683483, -49.56698729999997255, -99.89999999890753202 ) ) ;
#6035 = CARTESIAN_POINT ( 'NONE',  ( -25.99212434019154472, -33.65140427513057375, 7.988596311142242890 ) ) ;
#6036 = CARTESIAN_POINT ( 'NONE',  ( 5.000000000000000000, -47.07106781186545419, -97.04300000002184845 ) ) ;
#6037 = EDGE_CURVE ( 'NONE', #4798, #3552, #1155, .T. ) ;
#6038 = CARTESIAN_POINT ( 'NONE',  ( -23.68028341417693738, -39.75000000000000000, -6.319716585823200283 ) ) ;
#6039 = CARTESIAN_POINT ( 'NONE',  ( -3.061616997868382155E-16, -39.99999999999997158, -97.60000000000000853 ) ) ;
#6040 = CARTESIAN_POINT ( 'NONE',  ( -3.061616997868382155E-16, -39.99999999999997158, -95.89999999781505835 ) ) ;
#6041 = DIRECTION ( 'NONE',  ( 0.000000000000000000, 0.000000000000000000, 1.000000000000000000 ) ) ;
#6042 = ORIENTED_EDGE ( 'NONE', *, *, #6870, .T. ) ;
#6043 = FACE_BOUND ( 'NONE', #7020, .T. ) ;
#6044 = CARTESIAN_POINT ( 'NONE',  ( -22.93678734525658314, -42.75000000000001421, -7.063212654743582952 ) ) ;
#6045 = CARTESIAN_POINT ( 'NONE',  ( -21.16389173201424612, -48.05140427513057233, -1.343104241417630185 ) ) ;
#6046 = CIRCLE ( 'NONE', #8454, 1.000000000000000888 ) ;
#6047 = FACE_OUTER_BOUND ( 'NONE', #779, .T. ) ;
#6048 = LINE ( 'NONE', #7950, #8550 ) ;
#6049 = CARTESIAN_POINT ( 'NONE',  ( -28.46154767013959486, -47.79859572486944330, 9.374751783755112200 ) ) ;
#6050 = FACE_OUTER_BOUND ( 'NONE', #360, .T. ) ;
#6051 = DIRECTION ( 'NONE',  ( -1.000000000000000000, 0.000000000000000000, 0.000000000000000000 ) ) ;
#6052 = CARTESIAN_POINT ( 'NONE',  ( -3.229347689422840784, -41.77065231057713390, -98.74999999890751212 ) ) ;
#6053 =( LENGTH_UNIT ( ) NAMED_UNIT ( * ) SI_UNIT ( .MILLI., .METRE. ) );
#6054 = CONICAL_SURFACE ( 'NONE', #7318, 1.649999999999998579, 1.029744258676653645 ) ;
#6055 = VERTEX_POINT ( 'NONE', #4156 ) ;
#6056 = CARTESIAN_POINT ( 'NONE',  ( -17.99999999999998579, 1.469576158976828483E-15, -25.00000000000000000 ) ) ;
#6057 = CARTESIAN_POINT ( 'NONE',  ( -22.01140368885771892, -32.34859572486942625, 4.007875659808335378 ) ) ;
#6058 = CARTESIAN_POINT ( 'NONE',  ( -34.26570676250101855, -39.09859572486944046, 8.488613101951703044 ) ) ;
#6059 = CARTESIAN_POINT ( 'NONE',  ( -20.12537475255788522, -45.05140427513057944, -1.507589171976365439 ) ) ;
#6060 = EDGE_CURVE ( 'NONE', #4635, #912, #6834, .T. ) ;
#6061 = COLOUR_RGB ( '', 0.09019608, 0.27058824, 0.51372549) ;
#6062 = ORIENTED_EDGE ( 'NONE', *, *, #7316, .F. ) ;
#6063 = ORIENTED_EDGE ( 'NONE', *, *, #2221, .T. ) ;
#6064 = CARTESIAN_POINT ( 'NONE',  ( -38.87487832006816291, -46.85140427513056949, -4.584493831696867971 ) ) ;
#6065 = SURFACE_STYLE_FILL_AREA ( #3999 ) ;
#6066 = FACE_OUTER_BOUND ( 'NONE', #6433, .T. ) ;
#6067 = CARTESIAN_POINT ( 'NONE',  ( -3.535533905932736864, -41.46446609406723383, -98.99999999781503845 ) ) ;
#6068 = CARTESIAN_POINT ( 'NONE',  ( 34.99999999999998579, -44.99999999999995737, 11.45643923738957071 ) ) ;
#6069 = CARTESIAN_POINT ( 'NONE',  ( -4.999999999999998224, -42.92893218813448897, -99.85000000000002274 ) ) ;
#6070 = VERTEX_POINT ( 'NONE', #7104 ) ;
#6071 = CARTESIAN_POINT ( 'NONE',  ( -37.57355545560112375, -47.40000000000001279, 3.858919247786223305 ) ) ;
#6072 = ADVANCED_FACE ( 'NONE', ( #2355 ), #8344, .F. ) ;
#6073 = CARTESIAN_POINT ( 'NONE',  ( -21.09983283352784156, -34.35000000000000853, 4.534861676072186043 ) ) ;
#6074 = PRODUCT_DEFINITION_FORMATION_WITH_SPECIFIED_SOURCE ( 'ANY', '', #3813, .NOT_KNOWN. ) ;
#6075 = EDGE_LOOP ( 'NONE', ( #6817, #3911, #8534, #1278 ) ) ;
#6076 = CARTESIAN_POINT ( 'NONE',  ( -1.891708078845683039, -40.43301269999998482, -98.79999999890750928 ) ) ;
#6077 = CARTESIAN_POINT ( 'NONE',  ( 3.535533905932737309, -48.53553390593270933, -96.99999999781503845 ) ) ;
#6078 = CARTESIAN_POINT ( 'NONE',  ( -38.90016716647221529, -44.85000000000001563, -4.534861676072185155 ) ) ;
#6079 = CARTESIAN_POINT ( 'NONE',  ( 4.566987299999998307, -44.99999999999997158, -97.24999999890752633 ) ) ;
#6080 = FACE_OUTER_BOUND ( 'NONE', #8579, .T. ) ;
#6081 = CARTESIAN_POINT ( 'NONE',  ( -34.00787565980851213, -41.15140427513058086, -7.988596311142238449 ) ) ;
#6082 = VECTOR ( 'NONE', #4146, 1000.000000000000000 ) ;
#6083 = EDGE_CURVE ( 'NONE', #5819, #3280, #1016, .T. ) ;
#6084 = CARTESIAN_POINT ( 'NONE',  ( 5.000000000000000000, -47.07106781186545419, -97.84300000002187403 ) ) ;
#6085 =( GEOMETRIC_REPRESENTATION_CONTEXT ( 3 ) GLOBAL_UNCERTAINTY_ASSIGNED_CONTEXT ( ( #5459 ) ) GLOBAL_UNIT_ASSIGNED_CONTEXT ( ( #974, #841, #1591 ) ) REPRESENTATION_CONTEXT ( 'NONE', 'WORKASPACE' ) );
#6086 = CARTESIAN_POINT ( 'NONE',  ( -28.60187809025093841, -48.45000000000000284, -8.827394325379140483 ) ) ;
#6087 = CARTESIAN_POINT ( 'NONE',  ( 25.26672068143954064, -46.61962928414787655, 11.56930355017052037 ) ) ;
#6088 = DIRECTION ( 'NONE',  ( 0.000000000000000000, 0.000000000000000000, -1.000000000000000000 ) ) ;
#6089 = EDGE_LOOP ( 'NONE', ( #8297, #5657, #8715, #194 ) ) ;
#6090 = CYLINDRICAL_SURFACE ( 'NONE', #4600, 1.000000000000000888 ) ;
#6091 = AXIS2_PLACEMENT_3D ( 'NONE', #4067, #8126, #6088 ) ;
#6092 = CARTESIAN_POINT ( 'NONE',  ( -34.53486167607238144, -48.15000000000001279, -8.900167166472096270 ) ) ;
#6093 = CARTESIAN_POINT ( 'NONE',  ( -28.60187809025093841, -30.44999999999999574, -8.827394325379140483 ) ) ;
#6094 = FACE_OUTER_BOUND ( 'NONE', #4478, .T. ) ;
#6095 = CARTESIAN_POINT ( 'NONE',  ( -20.00000000000000355, 0.000000000000000000, 80.00000000000002842 ) ) ;
#6096 = CARTESIAN_POINT ( 'NONE',  ( -20.60867331244750034, -44.19859572486944899, 1.433802505903951419 ) ) ;
#6097 = CARTESIAN_POINT ( 'NONE',  ( -3.535533905932736864, -41.46446609406723383, -98.99999999781503845 ) ) ;
#6098 = CARTESIAN_POINT ( 'NONE',  ( 39.99999999999996447, 1.102182119232617753E-14, 80.00000000000002842 ) ) ;
#6099 = VERTEX_POINT ( 'NONE', #5033 ) ;
#6100 = DIRECTION ( 'NONE',  ( -0.000000000000000000, -0.000000000000000000, -1.000000000000000000 ) ) ;
#6101 = CARTESIAN_POINT ( 'NONE',  ( -28.60187809025093841, -48.44999999999999574, -8.827394325379140483 ) ) ;
#6102 = CARTESIAN_POINT ( 'NONE',  ( -28.49241082802385350, -40.44859572486944188, -9.874625247442173404 ) ) ;
#6103 = CARTESIAN_POINT ( 'NONE',  ( -28.56619749409589204, -45.80140427513057944, 9.391326687552490782 ) ) ;
#6104 = AXIS2_PLACEMENT_3D ( 'NONE', #3479, #1524, #6161 ) ;
#6105 = ORIENTED_EDGE ( 'NONE', *, *, #3009, .F. ) ;
#6106 = ADVANCED_FACE ( 'NONE', ( #3754 ), #4665, .T. ) ;
#6107 = ORIENTED_EDGE ( 'NONE', *, *, #4946, .F. ) ;
#6108 = CARTESIAN_POINT ( 'NONE',  ( -36.68005392025794009, -44.00140427513057517, -6.754974922286504757 ) ) ;
#6109 = CARTESIAN_POINT ( 'NONE',  ( -24.64110105645932336, -7.999999999999996447, -25.00000000000000000 ) ) ;
#6110 = CARTESIAN_POINT ( 'NONE',  ( -25.64110105645932336, -7.999999999999996447, 125.0000000000000000 ) ) ;
#6111 = CARTESIAN_POINT ( 'NONE',  ( 4.566987299999998307, -44.99999999999997158, -95.84999999890752065 ) ) ;
#6112 = DIRECTION ( 'NONE',  ( 0.000000000000000000, 0.5000000000000012212, 0.8660254037844380415 ) ) ;
#6113 = CARTESIAN_POINT ( 'NONE',  ( 42.00000000000000711, 48.00000000000002842, -21.99999999999992184 ) ) ;
#6114 = VECTOR ( 'NONE', #7102, 1000.000000000000000 ) ;
#6115 = ADVANCED_FACE ( 'NONE', ( #6395 ), #7143, .T. ) ;
#6116 = ORIENTED_EDGE ( 'NONE', *, *, #916, .T. ) ;
#6117 = CARTESIAN_POINT ( 'NONE',  ( -28.60187809025093841, -48.44999999999999574, -8.827394325379140483 ) ) ;
#6118 = CARTESIAN_POINT ( 'NONE',  ( -38.90016716647221529, -38.85000000000001563, -4.534861676072185155 ) ) ;
#6119 = ORIENTED_EDGE ( 'NONE', *, *, #5294, .T. ) ;
#6120 = DIRECTION ( 'NONE',  ( -1.000000000000000000, -0.000000000000000000, -0.000000000000000000 ) ) ;
#6121 = CARTESIAN_POINT ( 'NONE',  ( -4.566987299999998307, -43.10829192115428299, -97.09999999890752065 ) ) ;
#6122 = ADVANCED_FACE ( 'NONE', ( #5120 ), #3145, .T. ) ;
#6123 = CARTESIAN_POINT ( 'NONE',  ( 9.184850993605145972E-16, -49.99999999999997158, -97.89999999781504414 ) ) ;
#6124 = LINE ( 'NONE', #4187, #6082 ) ;
#6125 = CARTESIAN_POINT ( 'NONE',  ( 4.566987299999998307, -44.99999999999997158, -99.64999999890753202 ) ) ;
#6126 = CARTESIAN_POINT ( 'NONE',  ( -38.83610826798580717, -43.55140427513057944, 1.343104241417631073 ) ) ;
#6127 = EDGE_CURVE ( 'NONE', #4984, #5890, #1778, .T. ) ;
#6128 = CARTESIAN_POINT ( 'NONE',  ( -2.071067811865475505, -49.99999999999996447, -97.24300000002185129 ) ) ;
#6129 = CIRCLE ( 'NONE', #5712, 3.500000000000000000 ) ;
#6130 = CARTESIAN_POINT ( 'NONE',  ( -28.67030704715798350, -49.80000000000001137, 8.395350895058669494 ) ) ;
#6131 = ADVANCED_FACE ( 'NONE', ( #7058 ), #2480, .F. ) ;
#6132 = ADVANCED_FACE ( 'NONE', ( #7812 ), #6477, .T. ) ;
#6133 = CARTESIAN_POINT ( 'NONE',  ( -30.00000000000002842, 0.000000000000000000, -45.00000000000000000 ) ) ;
#6134 = PRODUCT_CONTEXT ( 'NONE', #4368, 'mechanical' ) ;
#6135 = ORIENTED_EDGE ( 'NONE', *, *, #4417, .T. ) ;
#6136 = CARTESIAN_POINT ( 'NONE',  ( 42.00000000000000711, 60.00000000000002842, 20.34999999999992326 ) ) ;
#6137 = CARTESIAN_POINT ( 'NONE',  ( -37.06321265474346660, -44.25000000000000000, 7.063212654743582952 ) ) ;
#6138 = CARTESIAN_POINT ( 'NONE',  ( -36.01040764008574513, -33.00000000000000711, -6.010407640085605685 ) ) ;
#6139 = VECTOR ( 'NONE', #2246, 1000.000000000000000 ) ;
#6140 =( BOUNDED_CURVE ( )  B_SPLINE_CURVE ( 2, ( #3533, #6211, #7574, #8163, #921, #4934, #1453, #7616, #258 ),
 .UNSPECIFIED., .F., .T. ) 
 B_SPLINE_CURVE_WITH_KNOTS ( ( 3, 2, 2, 2, 3 ),
 ( 0.3571428571428572063, 0.3750000000000000000, 0.3928571428571427937, 0.4107142857142856429, 0.4285714285714284366 ),
 .UNSPECIFIED. ) 
 CURVE ( )  GEOMETRIC_REPRESENTATION_ITEM ( )  RATIONAL_B_SPLINE_CURVE ( ( 0.9999999999999997780, 0.9238795325112869605, 1.000000000000000000, 0.9238795325112867385, 1.000000000000000000, 0.9238795325112867385, 1.000000000000000000, 0.9238795325112871826, 0.9999999999999995559 ) ) 
 REPRESENTATION_ITEM ( '' )  );
#6141 = DIRECTION ( 'NONE',  ( -0.000000000000000000, -0.000000000000000000, 1.000000000000000000 ) ) ;
#6142 = AXIS2_PLACEMENT_3D ( 'NONE', #6883, #4870, #7632 ) ;
#6143 = DIRECTION ( 'NONE',  ( 1.000000000000000000, 0.000000000000000000, 0.000000000000000000 ) ) ;
#6144 = CARTESIAN_POINT ( 'NONE',  ( -37.02382435302582309, -48.24859572486943904, 7.102600956461226467 ) ) ;
#6145 = CARTESIAN_POINT ( 'NONE',  ( 45.00000000000003553, -44.99999999999997158, 2.099999999999997868 ) ) ;
#6146 = CARTESIAN_POINT ( 'NONE',  ( -20.13408869516454303, -34.04999999999999005, -1.562606840307982692 ) ) ;
#6147 = VECTOR ( 'NONE', #4640, 1000.000000000000000 ) ;
#6148 = ORIENTED_EDGE ( 'NONE', *, *, #7316, .T. ) ;
#6149 = DIRECTION ( 'NONE',  ( -0.7061138087190598212, 0.05297714858780487590, 0.7061138087190823587 ) ) ;
#6150 = VERTEX_POINT ( 'NONE', #1683 ) ;
#6151 = CARTESIAN_POINT ( 'NONE',  ( -37.96330746473829976, -47.85000000000000853, -4.057507815433013754 ) ) ;
#6152 = CARTESIAN_POINT ( 'NONE',  ( -34.58449383169706692, -43.14859572486943762, -8.874878320068054549 ) ) ;
#6153 = CARTESIAN_POINT ( 'NONE',  ( -38.87487832006816291, -40.85140427513057659, -4.584493831696867971 ) ) ;
#6154 = ORIENTED_EDGE ( 'NONE', *, *, #7941, .T. ) ;
#6155 = CIRCLE ( 'NONE', #5590, 2.000000000000000888 ) ;
#6156 = VERTEX_POINT ( 'NONE', #3838 ) ;
#6157 = CARTESIAN_POINT ( 'NONE',  ( -2.796473189345805913E-16, -40.43301269999997061, -95.44999999890752918 ) ) ;
#6158 = EDGE_CURVE ( 'NONE', #4956, #4525, #6519, .T. ) ;
#6159 = CARTESIAN_POINT ( 'NONE',  ( -33.35889894354067309, -7.999999999999996447, 125.0000000000000000 ) ) ;
#6160 = CARTESIAN_POINT ( 'NONE',  ( -2.796473189345805913E-16, -40.43301269999997061, -96.44999999890751496 ) ) ;
#6161 = DIRECTION ( 'NONE',  ( -1.000000000000000000, 0.000000000000000000, 0.000000000000000000 ) ) ;
#6162 = DIRECTION ( 'NONE',  ( 0.000000000000000000, 0.000000000000000000, -1.000000000000000000 ) ) ;
#6163 = ORIENTED_EDGE ( 'NONE', *, *, #1743, .F. ) ;
#6164 = VECTOR ( 'NONE', #4502, 1000.000000000000000 ) ;
#6165 = CARTESIAN_POINT ( 'NONE',  ( -31.38201786482021305, -31.29859572486943975, -8.387063443159975762 ) ) ;
#6166 = CARTESIAN_POINT ( 'NONE',  ( -20.13408869516453947, -31.05000000000000782, -1.562606840307983136 ) ) ;
#6167 = VERTEX_POINT ( 'NONE', #471 ) ;
#6168 = CARTESIAN_POINT ( 'NONE',  ( -28.43739315969223824, -48.44999999999999574, -9.865911304835512041 ) ) ;
#6169 = CYLINDRICAL_SURFACE ( 'NONE', #5607, 4.999999999999998224 ) ;
#6170 = CARTESIAN_POINT ( 'NONE',  ( -4.566987299999997418, -46.89170807884566017, -98.59999999890753486 ) ) ;
#6171 = CARTESIAN_POINT ( 'NONE',  ( -3.535533905932735532, -48.53553390593270933, -99.59999999781504698 ) ) ;
#6172 = CYLINDRICAL_SURFACE ( 'NONE', #2436, 10.00000000000000178 ) ;
#6173 = CARTESIAN_POINT ( 'NONE',  ( -2.796473189345805913E-16, -40.43301269999997061, -98.64999999890753202 ) ) ;
#6174 = CARTESIAN_POINT ( 'NONE',  ( -21.61293655684001536, -39.20140427513058512, 1.382017864820032971 ) ) ;
#6175 = CARTESIAN_POINT ( 'NONE',  ( 3.535533905932737309, -48.53553390593270933, -95.50000000000000000 ) ) ;
#6176 = CARTESIAN_POINT ( 'NONE',  ( -38.39535089505872634, -47.70000000000000284, -1.329692952841885267 ) ) ;
#6177 = LINE ( 'NONE', #136, #8069 ) ;
#6178 = ORIENTED_EDGE ( 'NONE', *, *, #3043, .T. ) ;
#6179 = CARTESIAN_POINT ( 'NONE',  ( -44.14999999999995595, -22.00000000000000000, 60.00000000000002842 ) ) ;
#6180 = B_SPLINE_CURVE_WITH_KNOTS ( 'NONE', 3,
 ( #6813, #4840, #7560, #2284, #7476, #5620, #907, #6855, #4216, #7519, #3562, #4261, #8152, #1479, #1565, #6246, #3477, #6986, #4301, #3602 ),
 .UNSPECIFIED., .F., .F.,
 ( 4, 2, 2, 2, 2, 2, 2, 2, 2, 4 ),
 ( 0.007902764345171094454, 0.008889850383257352426, 0.009876936421343610398, 0.01086402245942986837, 0.01185110849751612634, 0.01283819453560238258, 0.01333173755464549942, 0.01382528057368861280, 0.01481236661177484301, 0.01579945264986107323 ),
 .UNSPECIFIED. ) ;
#6181 = CARTESIAN_POINT ( 'NONE',  ( -36.71751442127229836, -51.00000000000000711, -6.717514421272142044 ) ) ;
#6182 = CARTESIAN_POINT ( 'NONE',  ( -28.67030704715798350, -40.80000000000000426, 8.395350895058669494 ) ) ;
#6183 = CARTESIAN_POINT ( 'NONE',  ( -25.75674496862487572, -42.35030295949449197, 11.75814120956406050 ) ) ;
#6184 = CARTESIAN_POINT ( 'NONE',  ( 45.00000000000003553, -44.99999999999997158, -2.099999999999997868 ) ) ;
#6185 = CARTESIAN_POINT ( 'NONE',  ( -31.53845232986046554, -43.29859572486943620, -9.374751783755117529 ) ) ;
#6186 = DIRECTION ( 'NONE',  ( -0.7061138087190598212, 0.05297714858780487590, 0.7061138087190823587 ) ) ;
#6187 = CARTESIAN_POINT ( 'NONE',  ( -31.48612741788231517, -30.30000000000000782, -9.383039235653804155 ) ) ;
#6188 = ORIENTED_EDGE ( 'NONE', *, *, #1546, .T. ) ;
#6189 = DIRECTION ( 'NONE',  ( 0.000000000000000000, 1.000000000000000000, 0.000000000000000000 ) ) ;
#6190 = ORIENTED_EDGE ( 'NONE', *, *, #6608, .T. ) ;
#6191 = CARTESIAN_POINT ( 'NONE',  ( -21.18131961722757595, -38.04859572486944330, -1.453139578080854699 ) ) ;
#6192 = CARTESIAN_POINT ( 'NONE',  ( -31.50758917197619979, -38.94859572486943478, 9.874625247442176956 ) ) ;
#6193 = CARTESIAN_POINT ( 'NONE',  ( -38.48861310195163554, -37.40140427513058796, 4.265706762501153548 ) ) ;
#6194 = VECTOR ( 'NONE', #7504, 1000.000000000000114 ) ;
#6195 =( BOUNDED_SURFACE ( )  B_SPLINE_SURFACE ( 3, 2, ( 
 ( #8281, #1478, #6854, #4881, #2242, #4964, #4921, #7518, #2989, #7601, #115, #1564, #5664, #8367, #2330, #1162, #1875, #6494, #5708, #1752, #8528, #7078, #4434, #7159, #6367, #3164, #367, #404, #8488, #4391, #6536, #3812, #5175, #8571, #3117, #1119, #485, #8451, #7117, #1079, #3035, #3773, #445, #1791, #6452, #5795, #7868, #3076, #7243, #2453, #5134, #7201, #5838, #2494, #3730, #4560, #7826, #4473, #8410, #1037, #1204, #3857, #2535, #1832, #4514, #5214, #3201, #6411, #5884, #329, #2375, #7909, #5050, #7740, #1702, #7781, #5092, #5752, #2414, #7952, #7286, #1915, #5254, #8615, #3242, #4603, #3899, #6577, #531, #2584, #5924, #1530, #4359, #4271, #6334, #7039, #1668, #917, #3528, #3001, #211, #5495, #7614, #4313, #8379, #8248, #869, #124, #3572, #2823, #6256, #6206, #1487, #3487, #2914, #6908, #2165, #3612, #4224, #8205, #2870, #7659, #828, #6168, #170, #4850, #5542, #1621, #2207, #7528, #4892, #6995, #5584, #4183, #8291, #6864, #7569, #2251, #4930, #6292, #1577 ),
 ( #6953, #254, #2956, #5630, #8330, #2296, #4978, #960, #3655, #298, #5675, #2338, #5019, #7709, #4444, #1714, #5719, #2547, #7169, #7879, #378, #7795, #4572, #4401, #5144, #6421, #5849, #4527, #7836, #8421, #3085, #1129, #5223, #3824, #7089, #6504, #4483, #7127, #8460, #1762, #1047, #3739, #5185, #5763, #1090, #2423, #457, #7213, #1803, #8581, #3172, #3212, #2385, #3785, #8540, #2508, #3870, #1175, #2463, #7922, #1000, #1846, #6546, #5104, #499, #5896, #3698, #6462, #1888, #415, #6378, #338, #3045, #5059, #3128, #7749, #5807, #8501, #1216, #3432, #7433, #5394, #3302, #4746, #2060, #66, #7389, #588, #1390, #3912, #1967, #8052, #1343, #1298, #3253, #4085, #6763, #2015, #2109, #726, #6108, #2770, #6588, #543, #4614, #3998, #5438, #682, #7964, #2637, #4704, #7254, #4042, #1255, #6678, #635, #5264, #8150, #6723, #6064, #5934, #3343, #3387, #8628, #5976, #5309, #8011, #2595, #4656, #23, #2681, #7343, #6020, #2724, #3953, #1928, #8709, #5350, #8103, #7298, #6630 ),
 ( #8669, #3883, #2656, #8072, #2520, #1902, #4629, #3318, #4015, #4673, #2610, #3139, #1143, #5278, #7314, #8598, #7983, #1986, #3837, #5909, #7362, #516, #2033, #4720, #1944, #652, #2563, #5326, #7227, #6518, #470, #6035, #1315, #8026, #5241, #6694, #3362, #2698, #1270, #3227, #5367, #3184, #4587, #3970, #6649, #3929, #5865, #8556, #5196, #604, #7892, #1859, #4541, #1188, #6563, #7935, #7271, #6603, #1231, #559, #3270, #5992, #5951, #8644, #8683, #4061, #1407, #6213, #6174, #6739, #2128, #2790, #1456, #84, #5549, #2214, #5456, #3404, #791, #219, #698, #6081, #4190, #40, #6871, #2170, #6827, #4857, #8212, #745, #7533, #2922, #1493, #8121, #833, #3535, #4809, #6126, #8166, #7451, #4103, #2877, #4766, #7493, #4149, #178, #4899, #1360, #6781, #8255, #5594, #2743, #3493, #7577, #1538, #4232, #6915, #131, #6263, #7406, #2829, #877, #5503, #3580, #8298, #5411, #3449, #2259, #2078, #5816, #8508, #5728, #4451, #968, #386, #2303, #7619, #1584, #1099, #5110, #3092 ),
 ( #4985, #7135, #1676, #6960, #345, #5771, #3792, #3663, #2346, #4278, #5027, #924, #7717, #7667, #2965, #4938, #4366, #8386, #3620, #5068, #3008, #6302, #4322, #8469, #1629, #3137, #7005, #2431, #5683, #5638, #7050, #261, #8338, #6344, #306, #7758, #1010, #3706, #1722, #6386, #6469, #3053, #8428, #7803, #2392, #1770, #422, #4409, #7096, #1054, #3747, #6431, #6554, #3261, #2471, #7974, #5191, #5231, #4580, #464, #2647, #8636, #1261, #4663, #7928, #5941, #5316, #4536, #507, #3220, #7843, #7177, #7261, #4006, #1810, #1138, #1936, #3832, #4621, #2603, #1895, #5271, #7306, #3179, #4492, #3877, #1223, #6595, #5902, #5857, #6512, #6685, #3961, #596, #1853, #8588, #6028, #8548, #551, #7887, #6638, #2555, #2516, #3920, #3310, #5983, #8676, #8017, #1976, #7220, #3352, #7351, #1306, #643, #5154, #1184, #6071, #6904, #5445, #6770, #5358, #6731, #8245, #6117, #2204, #5492, #1445, #7566, #3525, #30, #4179, #3567, #4713, #8157, #121, #1351, #4799, #1398, #7440, #734, #866 ),
 ( #4094, #6203, #6165, #4138, #1527, #5401, #4221, #3440, #8339, #780, #2865, #2689, #8059, #2820, #2731, #4889, #2116, #2023, #6818, #825, #7396, #4755, #72, #4051, #2780, #690, #7481, #8110, #3396, #2069, #3483, #8202, #2160, #4846, #7525, #1484, #6861, #167, #5539, #4441, #2953, #1043, #4309, #6948, #5671, #7610, #1571, #5627, #913, #334, #8327, #4927, #3041, #8457, #1664, #2420, #6417, #8373, #2911, #251, #5056, #5016, #5581, #956, #1618, #294, #7655, #4397, #3736, #6992, #2248, #2335, #7790, #8288, #4266, #5716, #3608, #8417, #996, #7705, #3694, #7036, #6289, #2291, #3652, #4356, #6374, #6330, #4972, #2996, #1758, #2381, #7086, #7746, #1710, #1085, #374, #3082, #5759, #5100, #7124, #6252, #208, #5845, #3906, #5303, #6584, #4480, #539, #7249, #7208, #2503, #4522, #3819, #6499, #7959, #1126, #1169, #5181, #3250, #1251, #6459, #452, #5260, #1963, #5141, #3864, #1211, #5930, #6625, #7294, #5220, #2632, #3782, #7918, #8623, #7875, #1882, #4609, #411, #8536 ),
 ( #1841, #3949, #2591, #4567, #8006, #3169, #4651, #6542, #7338, #1921, #583, #3123, #5803, #3299, #493, #5973, #3207, #8497, #8665, #2459, #7833, #5892, #8577, #1798, #2543, #7166, #1385, #1339, #8048, #1294, #6757, #4742, #8704, #1430, #8098, #7469, #5434, #2852, #6718, #5528, #2056, #2191, #2104, #4168, #4877, #8232, #4126, #4038, #814, #720, #3338, #8144, #2148, #6192, #6058, #7428, #6674, #4081, #630, #3428, #677, #2010, #3994, #6102, #62, #2676, #6807, #2766, #6016, #3382, #5479, #7385, #5345, #18, #4834, #4786, #4700, #768, #2719, #5389, #3471, #6152, #110, #2808, #8188, #7513, #1474, #6849, #3515, #155, #5045, #901, #2369, #3071, #7691, #6892, #2941, #985, #8274, #5616, #8362, #7554, #4344, #1561, #1606, #944, #5567, #7735, #5003, #6362, #1033, #4296, #2238, #1517, #1697, #8317, #2280, #4210, #4961, #2325, #2985, #7643, #6980, #325, #4255, #8446, #3640, #6321, #8405, #1652, #3683, #4917, #5748, #284, #5659, #855, #7597, #7073, #7024, #3725, #3031 ),
 ( #2408, #3554, #5702, #4387, #198, #6407, #238, #6279, #362, #6238, #2900, #6938, #3599, #4553, #5170, #3806, #2578, #1786, #5960, #1827, #5833, #5918, #2530, #7237, #2449, #3282, #4508, #3158, #1747, #3109, #4597, #2488, #7281, #1869, #6531, #3936, #8608, #5130, #525, #8654, #1074, #7195, #5207, #6448, #1154, #6488, #438, #8522, #5087, #3893, #7776, #1197, #6572, #7862, #3849, #5249, #7903, #479, #6614, #4468, #569, #3194, #4430, #5877, #7946, #7112, #3767, #3236, #7821, #1240, #8566, #400, #1909, #5789, #8483, #1114, #7153, #7994, #6, #1952, #2707, #2665, #616, #2619, #8084, #6044, #1280, #2754, #664, #4637, #1996, #6792, #8692, #802, #8036, #6137, #3370, #3327, #2042, #3980, #6660, #4686, #6001, #5421, #7371, #5333, #8131, #1325, #4157, #4730, #3414, #97, #4026, #2796, #6835, #2091, #7325, #6703, #4774, #5376, #7415, #6092, #5288, #7459, #1373, #4070, #6746, #709, #5465, #50, #1417, #4817, #4113, #756, #3459, #8174, #2137, #7501, #1462, #3503, #6181 ) ),
 .UNSPECIFIED., .T., .F., .T. ) 
 B_SPLINE_SURFACE_WITH_KNOTS ( ( 4, 3, 4 ),
 ( 3, 2, 2, 2, 2, 2, 2, 2, 2, 2, 2, 2, 2, 2, 2, 2, 2, 2, 2, 2, 2, 2, 2, 2, 2, 2, 2, 2, 2, 2, 2, 2, 2, 2, 2, 2, 2, 2, 2, 2, 2, 2, 2, 2, 2, 2, 2, 2, 2, 2, 2, 2, 2, 2, 2, 2, 2, 2, 2, 2, 2, 2, 2, 2, 2, 2, 2, 2, 2, 2, 3 ),
 ( 0.000000000000000000, 0.5000000000000000000, 1.000000000000000000 ),
 ( 0.000000000000000000, 0.01428571428571428527, 0.02857142857142857054, 0.04285714285714285754, 0.05714285714285714107, 0.07142857142857142461, 0.08571428571428571508, 0.1000000000000000056, 0.1142857142857142821, 0.1285714285714285587, 0.1428571428571428492, 0.1571428571428571397, 0.1714285714285714302, 0.1857142857142857206, 0.2000000000000000111, 0.2142857142857142738, 0.2285714285714285643, 0.2428571428571428548, 0.2571428571428571175, 0.2714285714285714080, 0.2857142857142856984, 0.2999999999999999889, 0.3142857142857142794, 0.3285714285714285698, 0.3428571428571428603, 0.3571428571428571508, 0.3714285714285714413, 0.3857142857142857317, 0.4000000000000000222, 0.4142857142857143127, 0.4285714285714285476, 0.4428571428571428381, 0.4571428571428571286, 0.4714285714285714191, 0.4857142857142857095, 0.5000000000000000000, 0.5142857142857142350, 0.5285714285714285809, 0.5428571428571428159, 0.5571428571428571619, 0.5714285714285713969, 0.5857142857142857428, 0.5999999999999999778, 0.6142857142857143238, 0.6285714285714285587, 0.6428571428571429047, 0.6571428571428571397, 0.6714285714285713746, 0.6857142857142857206, 0.6999999999999999556, 0.7142857142857143016, 0.7285714285714285365, 0.7428571428571428825, 0.7571428571428571175, 0.7714285714285714635, 0.7857142857142856984, 0.8000000000000000444, 0.8142857142857142794, 0.8285714285714286254, 0.8428571428571428603, 0.8571428571428570953, 0.8714285714285714413, 0.8857142857142856762, 0.9000000000000000222, 0.9142857142857142572, 0.9285714285714286031, 0.9428571428571428381, 0.9571428571428571841, 0.9714285714285714191, 0.9857142857142857650, 1.000000000000000000 ),
 .UNSPECIFIED. ) 
 GEOMETRIC_REPRESENTATION_ITEM ( )  RATIONAL_B_SPLINE_SURFACE ( (
 ( 1.000000000000000000, 0.9510565162951535312, 1.000000000000000000, 0.9510565162951535312, 1.000000000000000000, 0.9510565162951535312, 1.000000000000000000, 0.9510565162951535312, 1.000000000000000000, 0.9510565162951535312, 1.000000000000000000, 0.9510565162951535312, 1.000000000000000000, 0.9510565162951535312, 1.000000000000000000, 0.9510565162951535312, 1.000000000000000000, 0.9510565162951535312, 1.000000000000000000, 0.9510565162951535312, 1.000000000000000000, 0.9510565162951535312, 1.000000000000000000, 0.9510565162951535312, 1.000000000000000000, 0.9510565162951535312, 1.000000000000000000, 0.9510565162951535312, 1.000000000000000000, 0.9510565162951535312, 1.000000000000000000, 0.9510565162951535312, 1.000000000000000000, 0.9510565162951535312, 1.000000000000000000, 0.9510565162951535312, 1.000000000000000000, 0.9510565162951535312, 1.000000000000000000, 0.9510565162951535312, 1.000000000000000000, 0.9510565162951535312, 1.000000000000000000, 0.9510565162951535312, 1.000000000000000000, 0.9510565162951535312, 1.000000000000000000, 0.9510565162951535312, 1.000000000000000000, 0.9510565162951535312, 1.000000000000000000, 0.9510565162951535312, 1.000000000000000000, 0.9510565162951535312, 1.000000000000000000, 0.9510565162951535312, 1.000000000000000000, 0.9510565162951535312, 1.000000000000000000, 0.9510565162951535312, 1.000000000000000000, 0.9510565162951535312, 1.000000000000000000, 0.9510565162951535312, 1.000000000000000000, 0.9510565162951535312, 1.000000000000000000, 0.9510565162951535312, 1.000000000000000000, 0.9510565162951535312, 1.000000000000000000, 0.9510565162951535312, 1.000000000000000000, 0.9510565162951535312, 1.000000000000000000, 0.9510565162951535312, 1.000000000000000000, 0.9510565162951535312, 1.000000000000000000, 0.9510565162951535312, 1.000000000000000000, 0.9510565162951535312, 1.000000000000000000, 0.9510565162951535312, 1.000000000000000000, 0.9510565162951535312, 1.000000000000000000, 0.9510565162951535312, 1.000000000000000000, 0.9510565162951535312, 1.000000000000000000, 0.9510565162951535312, 1.000000000000000000, 0.9510565162951535312, 1.000000000000000000, 0.9510565162951535312, 1.000000000000000000, 0.9510565162951535312, 1.000000000000000000, 0.9510565162951535312, 1.000000000000000000, 0.9510565162951535312, 1.000000000000000000, 0.9510565162951535312, 1.000000000000000000, 0.9510565162951535312, 1.000000000000000000, 0.9510565162951535312, 1.000000000000000000, 0.9510565162951535312, 1.000000000000000000, 0.9510565162951535312, 1.000000000000000000, 0.9510565162951535312, 1.000000000000000000, 0.9510565162951535312, 1.000000000000000000, 0.9510565162951535312, 1.000000000000000000, 0.9510565162951535312, 1.000000000000000000, 0.9510565162951535312, 1.000000000000000000, 0.9510565162951535312, 1.000000000000000000, 0.9510565162951535312, 1.000000000000000000, 0.9510565162951535312, 1.000000000000000000, 0.9510565162951535312, 1.000000000000000000, 0.9510565162951535312, 1.000000000000000000, 0.9510565162951535312, 1.000000000000000000, 0.9510565162951535312, 1.000000000000000000, 0.9510565162951535312, 1.000000000000000000, 0.9510565162951535312, 1.000000000000000000),
 ( 0.3333333333333333703, 0.3170188387650512141, 0.3333333333333333703, 0.3170188387650512141, 0.3333333333333333703, 0.3170188387650512141, 0.3333333333333333703, 0.3170188387650512141, 0.3333333333333333703, 0.3170188387650512141, 0.3333333333333333703, 0.3170188387650512141, 0.3333333333333333703, 0.3170188387650512141, 0.3333333333333333703, 0.3170188387650512141, 0.3333333333333333703, 0.3170188387650512141, 0.3333333333333333703, 0.3170188387650512141, 0.3333333333333333703, 0.3170188387650512141, 0.3333333333333333703, 0.3170188387650512141, 0.3333333333333333703, 0.3170188387650512141, 0.3333333333333333703, 0.3170188387650512141, 0.3333333333333333703, 0.3170188387650512141, 0.3333333333333333703, 0.3170188387650512141, 0.3333333333333333703, 0.3170188387650512141, 0.3333333333333333703, 0.3170188387650512141, 0.3333333333333333703, 0.3170188387650512141, 0.3333333333333333703, 0.3170188387650512141, 0.3333333333333333703, 0.3170188387650512141, 0.3333333333333333703, 0.3170188387650512141, 0.3333333333333333703, 0.3170188387650512141, 0.3333333333333333703, 0.3170188387650512141, 0.3333333333333333703, 0.3170188387650512141, 0.3333333333333333703, 0.3170188387650512141, 0.3333333333333333703, 0.3170188387650512141, 0.3333333333333333703, 0.3170188387650512141, 0.3333333333333333703, 0.3170188387650512141, 0.3333333333333333703, 0.3170188387650512141, 0.3333333333333333703, 0.3170188387650512141, 0.3333333333333333703, 0.3170188387650512141, 0.3333333333333333703, 0.3170188387650512141, 0.3333333333333333703, 0.3170188387650512141, 0.3333333333333333703, 0.3170188387650512141, 0.3333333333333333703, 0.3170188387650512141, 0.3333333333333333703, 0.3170188387650512141, 0.3333333333333333703, 0.3170188387650512141, 0.3333333333333333703, 0.3170188387650512141, 0.3333333333333333703, 0.3170188387650512141, 0.3333333333333333703, 0.3170188387650512141, 0.3333333333333333703, 0.3170188387650512141, 0.3333333333333333703, 0.3170188387650512141, 0.3333333333333333703, 0.3170188387650512141, 0.3333333333333333703, 0.3170188387650512141, 0.3333333333333333703, 0.3170188387650512141, 0.3333333333333333703, 0.3170188387650512141, 0.3333333333333333703, 0.3170188387650512141, 0.3333333333333333703, 0.3170188387650512141, 0.3333333333333333703, 0.3170188387650512141, 0.3333333333333333703, 0.3170188387650512141, 0.3333333333333333703, 0.3170188387650512141, 0.3333333333333333703, 0.3170188387650512141, 0.3333333333333333703, 0.3170188387650512141, 0.3333333333333333703, 0.3170188387650512141, 0.3333333333333333703, 0.3170188387650512141, 0.3333333333333333703, 0.3170188387650512141, 0.3333333333333333703, 0.3170188387650512141, 0.3333333333333333703, 0.3170188387650512141, 0.3333333333333333703, 0.3170188387650512141, 0.3333333333333333703, 0.3170188387650512141, 0.3333333333333333703, 0.3170188387650512141, 0.3333333333333333703, 0.3170188387650512141, 0.3333333333333333703, 0.3170188387650512141, 0.3333333333333333703, 0.3170188387650512141, 0.3333333333333333703, 0.3170188387650512141, 0.3333333333333333703, 0.3170188387650512141, 0.3333333333333333703, 0.3170188387650512141, 0.3333333333333333703, 0.3170188387650512141, 0.3333333333333333703, 0.3170188387650512141, 0.3333333333333333703),
 ( 0.3333333333333333703, 0.3170188387650512141, 0.3333333333333333703, 0.3170188387650512141, 0.3333333333333333703, 0.3170188387650512141, 0.3333333333333333703, 0.3170188387650512141, 0.3333333333333333703, 0.3170188387650512141, 0.3333333333333333703, 0.3170188387650512141, 0.3333333333333333703, 0.3170188387650512141, 0.3333333333333333703, 0.3170188387650512141, 0.3333333333333333703, 0.3170188387650512141, 0.3333333333333333703, 0.3170188387650512141, 0.3333333333333333703, 0.3170188387650512141, 0.3333333333333333703, 0.3170188387650512141, 0.3333333333333333703, 0.3170188387650512141, 0.3333333333333333703, 0.3170188387650512141, 0.3333333333333333703, 0.3170188387650512141, 0.3333333333333333703, 0.3170188387650512141, 0.3333333333333333703, 0.3170188387650512141, 0.3333333333333333703, 0.3170188387650512141, 0.3333333333333333703, 0.3170188387650512141, 0.3333333333333333703, 0.3170188387650512141, 0.3333333333333333703, 0.3170188387650512141, 0.3333333333333333703, 0.3170188387650512141, 0.3333333333333333703, 0.3170188387650512141, 0.3333333333333333703, 0.3170188387650512141, 0.3333333333333333703, 0.3170188387650512141, 0.3333333333333333703, 0.3170188387650512141, 0.3333333333333333703, 0.3170188387650512141, 0.3333333333333333703, 0.3170188387650512141, 0.3333333333333333703, 0.3170188387650512141, 0.3333333333333333703, 0.3170188387650512141, 0.3333333333333333703, 0.3170188387650512141, 0.3333333333333333703, 0.3170188387650512141, 0.3333333333333333703, 0.3170188387650512141, 0.3333333333333333703, 0.3170188387650512141, 0.3333333333333333703, 0.3170188387650512141, 0.3333333333333333703, 0.3170188387650512141, 0.3333333333333333703, 0.3170188387650512141, 0.3333333333333333703, 0.3170188387650512141, 0.3333333333333333703, 0.3170188387650512141, 0.3333333333333333703, 0.3170188387650512141, 0.3333333333333333703, 0.3170188387650512141, 0.3333333333333333703, 0.3170188387650512141, 0.3333333333333333703, 0.3170188387650512141, 0.3333333333333333703, 0.3170188387650512141, 0.3333333333333333703, 0.3170188387650512141, 0.3333333333333333703, 0.3170188387650512141, 0.3333333333333333703, 0.3170188387650512141, 0.3333333333333333703, 0.3170188387650512141, 0.3333333333333333703, 0.3170188387650512141, 0.3333333333333333703, 0.3170188387650512141, 0.3333333333333333703, 0.3170188387650512141, 0.3333333333333333703, 0.3170188387650512141, 0.3333333333333333703, 0.3170188387650512141, 0.3333333333333333703, 0.3170188387650512141, 0.3333333333333333703, 0.3170188387650512141, 0.3333333333333333703, 0.3170188387650512141, 0.3333333333333333703, 0.3170188387650512141, 0.3333333333333333703, 0.3170188387650512141, 0.3333333333333333703, 0.3170188387650512141, 0.3333333333333333703, 0.3170188387650512141, 0.3333333333333333703, 0.3170188387650512141, 0.3333333333333333703, 0.3170188387650512141, 0.3333333333333333703, 0.3170188387650512141, 0.3333333333333333703, 0.3170188387650512141, 0.3333333333333333703, 0.3170188387650512141, 0.3333333333333333703, 0.3170188387650512141, 0.3333333333333333703, 0.3170188387650512141, 0.3333333333333333703, 0.3170188387650512141, 0.3333333333333333703, 0.3170188387650512141, 0.3333333333333333703, 0.3170188387650512141, 0.3333333333333333703),
 ( 1.000000000000000000, 0.9510565162951535312, 1.000000000000000000, 0.9510565162951535312, 1.000000000000000000, 0.9510565162951535312, 1.000000000000000000, 0.9510565162951535312, 1.000000000000000000, 0.9510565162951535312, 1.000000000000000000, 0.9510565162951535312, 1.000000000000000000, 0.9510565162951535312, 1.000000000000000000, 0.9510565162951535312, 1.000000000000000000, 0.9510565162951535312, 1.000000000000000000, 0.9510565162951535312, 1.000000000000000000, 0.9510565162951535312, 1.000000000000000000, 0.9510565162951535312, 1.000000000000000000, 0.9510565162951535312, 1.000000000000000000, 0.9510565162951535312, 1.000000000000000000, 0.9510565162951535312, 1.000000000000000000, 0.9510565162951535312, 1.000000000000000000, 0.9510565162951535312, 1.000000000000000000, 0.9510565162951535312, 1.000000000000000000, 0.9510565162951535312, 1.000000000000000000, 0.9510565162951535312, 1.000000000000000000, 0.9510565162951535312, 1.000000000000000000, 0.9510565162951535312, 1.000000000000000000, 0.9510565162951535312, 1.000000000000000000, 0.9510565162951535312, 1.000000000000000000, 0.9510565162951535312, 1.000000000000000000, 0.9510565162951535312, 1.000000000000000000, 0.9510565162951535312, 1.000000000000000000, 0.9510565162951535312, 1.000000000000000000, 0.9510565162951535312, 1.000000000000000000, 0.9510565162951535312, 1.000000000000000000, 0.9510565162951535312, 1.000000000000000000, 0.9510565162951535312, 1.000000000000000000, 0.9510565162951535312, 1.000000000000000000, 0.9510565162951535312, 1.000000000000000000, 0.9510565162951535312, 1.000000000000000000, 0.9510565162951535312, 1.000000000000000000, 0.9510565162951535312, 1.000000000000000000, 0.9510565162951535312, 1.000000000000000000, 0.9510565162951535312, 1.000000000000000000, 0.9510565162951535312, 1.000000000000000000, 0.9510565162951535312, 1.000000000000000000, 0.9510565162951535312, 1.000000000000000000, 0.9510565162951535312, 1.000000000000000000, 0.9510565162951535312, 1.000000000000000000, 0.9510565162951535312, 1.000000000000000000, 0.9510565162951535312, 1.000000000000000000, 0.9510565162951535312, 1.000000000000000000, 0.9510565162951535312, 1.000000000000000000, 0.9510565162951535312, 1.000000000000000000, 0.9510565162951535312, 1.000000000000000000, 0.9510565162951535312, 1.000000000000000000, 0.9510565162951535312, 1.000000000000000000, 0.9510565162951535312, 1.000000000000000000, 0.9510565162951535312, 1.000000000000000000, 0.9510565162951535312, 1.000000000000000000, 0.9510565162951535312, 1.000000000000000000, 0.9510565162951535312, 1.000000000000000000, 0.9510565162951535312, 1.000000000000000000, 0.9510565162951535312, 1.000000000000000000, 0.9510565162951535312, 1.000000000000000000, 0.9510565162951535312, 1.000000000000000000, 0.9510565162951535312, 1.000000000000000000, 0.9510565162951535312, 1.000000000000000000, 0.9510565162951535312, 1.000000000000000000, 0.9510565162951535312, 1.000000000000000000, 0.9510565162951535312, 1.000000000000000000, 0.9510565162951535312, 1.000000000000000000, 0.9510565162951535312, 1.000000000000000000, 0.9510565162951535312, 1.000000000000000000, 0.9510565162951535312, 1.000000000000000000),
 ( 0.3333333333333333703, 0.3170188387650512141, 0.3333333333333333703, 0.3170188387650512141, 0.3333333333333333703, 0.3170188387650512141, 0.3333333333333333703, 0.3170188387650512141, 0.3333333333333333703, 0.3170188387650512141, 0.3333333333333333703, 0.3170188387650512141, 0.3333333333333333703, 0.3170188387650512141, 0.3333333333333333703, 0.3170188387650512141, 0.3333333333333333703, 0.3170188387650512141, 0.3333333333333333703, 0.3170188387650512141, 0.3333333333333333703, 0.3170188387650512141, 0.3333333333333333703, 0.3170188387650512141, 0.3333333333333333703, 0.3170188387650512141, 0.3333333333333333703, 0.3170188387650512141, 0.3333333333333333703, 0.3170188387650512141, 0.3333333333333333703, 0.3170188387650512141, 0.3333333333333333703, 0.3170188387650512141, 0.3333333333333333703, 0.3170188387650512141, 0.3333333333333333703, 0.3170188387650512141, 0.3333333333333333703, 0.3170188387650512141, 0.3333333333333333703, 0.3170188387650512141, 0.3333333333333333703, 0.3170188387650512141, 0.3333333333333333703, 0.3170188387650512141, 0.3333333333333333703, 0.3170188387650512141, 0.3333333333333333703, 0.3170188387650512141, 0.3333333333333333703, 0.3170188387650512141, 0.3333333333333333703, 0.3170188387650512141, 0.3333333333333333703, 0.3170188387650512141, 0.3333333333333333703, 0.3170188387650512141, 0.3333333333333333703, 0.3170188387650512141, 0.3333333333333333703, 0.3170188387650512141, 0.3333333333333333703, 0.3170188387650512141, 0.3333333333333333703, 0.3170188387650512141, 0.3333333333333333703, 0.3170188387650512141, 0.3333333333333333703, 0.3170188387650512141, 0.3333333333333333703, 0.3170188387650512141, 0.3333333333333333703, 0.3170188387650512141, 0.3333333333333333703, 0.3170188387650512141, 0.3333333333333333703, 0.3170188387650512141, 0.3333333333333333703, 0.3170188387650512141, 0.3333333333333333703, 0.3170188387650512141, 0.3333333333333333703, 0.3170188387650512141, 0.3333333333333333703, 0.3170188387650512141, 0.3333333333333333703, 0.3170188387650512141, 0.3333333333333333703, 0.3170188387650512141, 0.3333333333333333703, 0.3170188387650512141, 0.3333333333333333703, 0.3170188387650512141, 0.3333333333333333703, 0.3170188387650512141, 0.3333333333333333703, 0.3170188387650512141, 0.3333333333333333703, 0.3170188387650512141, 0.3333333333333333703, 0.3170188387650512141, 0.3333333333333333703, 0.3170188387650512141, 0.3333333333333333703, 0.3170188387650512141, 0.3333333333333333703, 0.3170188387650512141, 0.3333333333333333703, 0.3170188387650512141, 0.3333333333333333703, 0.3170188387650512141, 0.3333333333333333703, 0.3170188387650512141, 0.3333333333333333703, 0.3170188387650512141, 0.3333333333333333703, 0.3170188387650512141, 0.3333333333333333703, 0.3170188387650512141, 0.3333333333333333703, 0.3170188387650512141, 0.3333333333333333703, 0.3170188387650512141, 0.3333333333333333703, 0.3170188387650512141, 0.3333333333333333703, 0.3170188387650512141, 0.3333333333333333703, 0.3170188387650512141, 0.3333333333333333703, 0.3170188387650512141, 0.3333333333333333703, 0.3170188387650512141, 0.3333333333333333703, 0.3170188387650512141, 0.3333333333333333703, 0.3170188387650512141, 0.3333333333333333703, 0.3170188387650512141, 0.3333333333333333703),
 ( 0.3333333333333333703, 0.3170188387650512141, 0.3333333333333333703, 0.3170188387650512141, 0.3333333333333333703, 0.3170188387650512141, 0.3333333333333333703, 0.3170188387650512141, 0.3333333333333333703, 0.3170188387650512141, 0.3333333333333333703, 0.3170188387650512141, 0.3333333333333333703, 0.3170188387650512141, 0.3333333333333333703, 0.3170188387650512141, 0.3333333333333333703, 0.3170188387650512141, 0.3333333333333333703, 0.3170188387650512141, 0.3333333333333333703, 0.3170188387650512141, 0.3333333333333333703, 0.3170188387650512141, 0.3333333333333333703, 0.3170188387650512141, 0.3333333333333333703, 0.3170188387650512141, 0.3333333333333333703, 0.3170188387650512141, 0.3333333333333333703, 0.3170188387650512141, 0.3333333333333333703, 0.3170188387650512141, 0.3333333333333333703, 0.3170188387650512141, 0.3333333333333333703, 0.3170188387650512141, 0.3333333333333333703, 0.3170188387650512141, 0.3333333333333333703, 0.3170188387650512141, 0.3333333333333333703, 0.3170188387650512141, 0.3333333333333333703, 0.3170188387650512141, 0.3333333333333333703, 0.3170188387650512141, 0.3333333333333333703, 0.3170188387650512141, 0.3333333333333333703, 0.3170188387650512141, 0.3333333333333333703, 0.3170188387650512141, 0.3333333333333333703, 0.3170188387650512141, 0.3333333333333333703, 0.3170188387650512141, 0.3333333333333333703, 0.3170188387650512141, 0.3333333333333333703, 0.3170188387650512141, 0.3333333333333333703, 0.3170188387650512141, 0.3333333333333333703, 0.3170188387650512141, 0.3333333333333333703, 0.3170188387650512141, 0.3333333333333333703, 0.3170188387650512141, 0.3333333333333333703, 0.3170188387650512141, 0.3333333333333333703, 0.3170188387650512141, 0.3333333333333333703, 0.3170188387650512141, 0.3333333333333333703, 0.3170188387650512141, 0.3333333333333333703, 0.3170188387650512141, 0.3333333333333333703, 0.3170188387650512141, 0.3333333333333333703, 0.3170188387650512141, 0.3333333333333333703, 0.3170188387650512141, 0.3333333333333333703, 0.3170188387650512141, 0.3333333333333333703, 0.3170188387650512141, 0.3333333333333333703, 0.3170188387650512141, 0.3333333333333333703, 0.3170188387650512141, 0.3333333333333333703, 0.3170188387650512141, 0.3333333333333333703, 0.3170188387650512141, 0.3333333333333333703, 0.3170188387650512141, 0.3333333333333333703, 0.3170188387650512141, 0.3333333333333333703, 0.3170188387650512141, 0.3333333333333333703, 0.3170188387650512141, 0.3333333333333333703, 0.3170188387650512141, 0.3333333333333333703, 0.3170188387650512141, 0.3333333333333333703, 0.3170188387650512141, 0.3333333333333333703, 0.3170188387650512141, 0.3333333333333333703, 0.3170188387650512141, 0.3333333333333333703, 0.3170188387650512141, 0.3333333333333333703, 0.3170188387650512141, 0.3333333333333333703, 0.3170188387650512141, 0.3333333333333333703, 0.3170188387650512141, 0.3333333333333333703, 0.3170188387650512141, 0.3333333333333333703, 0.3170188387650512141, 0.3333333333333333703, 0.3170188387650512141, 0.3333333333333333703, 0.3170188387650512141, 0.3333333333333333703, 0.3170188387650512141, 0.3333333333333333703, 0.3170188387650512141, 0.3333333333333333703, 0.3170188387650512141, 0.3333333333333333703, 0.3170188387650512141, 0.3333333333333333703),
 ( 1.000000000000000000, 0.9510565162951535312, 1.000000000000000000, 0.9510565162951535312, 1.000000000000000000, 0.9510565162951535312, 1.000000000000000000, 0.9510565162951535312, 1.000000000000000000, 0.9510565162951535312, 1.000000000000000000, 0.9510565162951535312, 1.000000000000000000, 0.9510565162951535312, 1.000000000000000000, 0.9510565162951535312, 1.000000000000000000, 0.9510565162951535312, 1.000000000000000000, 0.9510565162951535312, 1.000000000000000000, 0.9510565162951535312, 1.000000000000000000, 0.9510565162951535312, 1.000000000000000000, 0.9510565162951535312, 1.000000000000000000, 0.9510565162951535312, 1.000000000000000000, 0.9510565162951535312, 1.000000000000000000, 0.9510565162951535312, 1.000000000000000000, 0.9510565162951535312, 1.000000000000000000, 0.9510565162951535312, 1.000000000000000000, 0.9510565162951535312, 1.000000000000000000, 0.9510565162951535312, 1.000000000000000000, 0.9510565162951535312, 1.000000000000000000, 0.9510565162951535312, 1.000000000000000000, 0.9510565162951535312, 1.000000000000000000, 0.9510565162951535312, 1.000000000000000000, 0.9510565162951535312, 1.000000000000000000, 0.9510565162951535312, 1.000000000000000000, 0.9510565162951535312, 1.000000000000000000, 0.9510565162951535312, 1.000000000000000000, 0.9510565162951535312, 1.000000000000000000, 0.9510565162951535312, 1.000000000000000000, 0.9510565162951535312, 1.000000000000000000, 0.9510565162951535312, 1.000000000000000000, 0.9510565162951535312, 1.000000000000000000, 0.9510565162951535312, 1.000000000000000000, 0.9510565162951535312, 1.000000000000000000, 0.9510565162951535312, 1.000000000000000000, 0.9510565162951535312, 1.000000000000000000, 0.9510565162951535312, 1.000000000000000000, 0.9510565162951535312, 1.000000000000000000, 0.9510565162951535312, 1.000000000000000000, 0.9510565162951535312, 1.000000000000000000, 0.9510565162951535312, 1.000000000000000000, 0.9510565162951535312, 1.000000000000000000, 0.9510565162951535312, 1.000000000000000000, 0.9510565162951535312, 1.000000000000000000, 0.9510565162951535312, 1.000000000000000000, 0.9510565162951535312, 1.000000000000000000, 0.9510565162951535312, 1.000000000000000000, 0.9510565162951535312, 1.000000000000000000, 0.9510565162951535312, 1.000000000000000000, 0.9510565162951535312, 1.000000000000000000, 0.9510565162951535312, 1.000000000000000000, 0.9510565162951535312, 1.000000000000000000, 0.9510565162951535312, 1.000000000000000000, 0.9510565162951535312, 1.000000000000000000, 0.9510565162951535312, 1.000000000000000000, 0.9510565162951535312, 1.000000000000000000, 0.9510565162951535312, 1.000000000000000000, 0.9510565162951535312, 1.000000000000000000, 0.9510565162951535312, 1.000000000000000000, 0.9510565162951535312, 1.000000000000000000, 0.9510565162951535312, 1.000000000000000000, 0.9510565162951535312, 1.000000000000000000, 0.9510565162951535312, 1.000000000000000000, 0.9510565162951535312, 1.000000000000000000, 0.9510565162951535312, 1.000000000000000000, 0.9510565162951535312, 1.000000000000000000, 0.9510565162951535312, 1.000000000000000000, 0.9510565162951535312, 1.000000000000000000, 0.9510565162951535312, 1.000000000000000000) ) ) 
 REPRESENTATION_ITEM ( '' )  SURFACE ( )  );
#6196 = ORIENTED_EDGE ( 'NONE', *, *, #7701, .F. ) ;
#6197 = CARTESIAN_POINT ( 'NONE',  ( 1.891708078845685481, -49.56698729999997255, -96.59999999890754907 ) ) ;
#6198 = LINE ( 'NONE', #5486, #1361 ) ;
#6199 = CARTESIAN_POINT ( 'NONE',  ( 4.566987299999998307, -44.99999999999997158, -98.24999999890751212 ) ) ;
#6200 = DIRECTION ( 'NONE',  ( -0.000000000000000000, -0.000000000000000000, 1.000000000000000000 ) ) ;
#6201 = FACE_OUTER_BOUND ( 'NONE', #625, .T. ) ;
#6202 = ORIENTED_EDGE ( 'NONE', *, *, #612, .T. ) ;
#6203 = CARTESIAN_POINT ( 'NONE',  ( -34.10713997105786888, -31.14859572486944828, -7.938018618334151455 ) ) ;
#6204 = CARTESIAN_POINT ( 'NONE',  ( -28.43739315969223824, -30.44999999999999574, -9.865911304835512041 ) ) ;
#6205 = ORIENTED_EDGE ( 'NONE', *, *, #4675, .F. ) ;
#6206 = CARTESIAN_POINT ( 'NONE',  ( -25.46513832392765408, -46.65000000000001279, 8.900167166472096270 ) ) ;
#6207 = CARTESIAN_POINT ( 'NONE',  ( 9.184850993605145972E-16, -49.99999999999997158, -98.69999999781505551 ) ) ;
#6208 = CARTESIAN_POINT ( 'NONE',  ( -4.566987299999998307, -43.10829192115428299, -99.49999999890752633 ) ) ;
#6209 = CARTESIAN_POINT ( 'NONE',  ( -4.999999999999997335, -47.07106781186546129, -98.84999999781503277 ) ) ;
#6210 = VECTOR ( 'NONE', #1230, 1000.000000000000000 ) ;
#6211 = CARTESIAN_POINT ( 'NONE',  ( 4.999999999999994671, -47.07106781186546129, -97.74999999781505267 ) ) ;
#6212 = CARTESIAN_POINT ( 'NONE',  ( 4.566987300000000083, -46.89170807884565306, -98.89999999890753202 ) ) ;
#6213 = CARTESIAN_POINT ( 'NONE',  ( -21.16389173201424612, -39.05140427513057944, -1.343104241417630185 ) ) ;
#6214 = COLOUR_RGB ( '', 0.31764706, 0.68627451, 0.89019608) ;
#6215 = CARTESIAN_POINT ( 'NONE',  ( -4.999999999999998224, -44.99999999999997158, -98.99300000002185129 ) ) ;
#6216 = APPLICATION_CONTEXT ( 'automotive_design' ) ;
#6217 = CARTESIAN_POINT ( 'NONE',  ( 3.229347689422841228, -48.22934768942280925, -96.54999999890752349 ) ) ;
#6218 = CARTESIAN_POINT ( 'NONE',  ( -28.60187809025093841, -45.45000000000000284, -8.827394325379140483 ) ) ;
#6219 = CARTESIAN_POINT ( 'NONE',  ( 4.566987299999998307, -43.10829192115428299, -96.59999999890753486 ) ) ;
#6220 = FACE_OUTER_BOUND ( 'NONE', #5263, .T. ) ;
#6221 = APPLICATION_PROTOCOL_DEFINITION ( 'draft international standard', 'automotive_design', 1998, #6332 ) ;
#6222 = CARTESIAN_POINT ( 'NONE',  ( -41.99999999999996447, 48.00000000000002842, -22.00000000000000000 ) ) ;
#6223 = EDGE_CURVE ( 'NONE', #4124, #5183, #350, .T. ) ;
#6224 = CARTESIAN_POINT ( 'NONE',  ( -37.57355545560112375, -38.40000000000000568, 3.858919247786223305 ) ) ;
#6225 = VECTOR ( 'NONE', #2874, 1000.000000000000000 ) ;
#6226 = CARTESIAN_POINT ( 'NONE',  ( 28.68975157273829169, -40.16330870357082716, 12.43543189630222656 ) ) ;
#6227 = DIRECTION ( 'NONE',  ( -0.000000000000000000, -0.000000000000000000, 1.000000000000000000 ) ) ;
#6228 = CARTESIAN_POINT ( 'NONE',  ( -31.50758917197619979, -44.94859572486942767, 9.874625247442176956 ) ) ;
#6229 = ADVANCED_FACE ( 'NONE', ( #5866 ), #5660, .F. ) ;
#6230 = LINE ( 'NONE', #2846, #3946 ) ;
#6231 = CARTESIAN_POINT ( 'NONE',  ( -20.61696076434619584, -31.20000000000000639, 1.486127417882100676 ) ) ;
#6232 = FILL_AREA_STYLE_COLOUR ( '', #2140 ) ;
#6233 = ORIENTED_EDGE ( 'NONE', *, *, #3138, .T. ) ;
#6234 = CARTESIAN_POINT ( 'NONE',  ( 42.00000000000000711, 21.99999999999992184, 80.00000000000002842 ) ) ;
#6235 = VERTEX_POINT ( 'NONE', #2521 ) ;
#6236 = VECTOR ( 'NONE', #1132, 1000.000000000000000 ) ;
#6237 = CARTESIAN_POINT ( 'NONE',  ( -36.04786814110010340, -42.99859572486943904, -5.972947139071243861 ) ) ;
#6238 = CARTESIAN_POINT ( 'NONE',  ( -21.09983283352784156, -31.34999999999999787, 4.534861676072186043 ) ) ;
#6239 = CARTESIAN_POINT ( 'NONE',  ( -21.12512167993187973, -48.35140427513057659, 4.584493831696868860 ) ) ;
#6240 = ADVANCED_FACE ( 'NONE', ( #8557 ), #5074, .T. ) ;
#6241 = ORIENTED_EDGE ( 'NONE', *, *, #8591, .T. ) ;
#6242 = CARTESIAN_POINT ( 'NONE',  ( 3.229347689422839895, -41.77065231057713390, -95.54999999890752349 ) ) ;
#6243 = CIRCLE ( 'NONE', #7363, 2.000000000000001776 ) ;
#6244 = DIRECTION ( 'NONE',  ( 0.000000000000000000, 0.000000000000000000, 1.000000000000000000 ) ) ;
#6245 = PRODUCT_DEFINITION_SHAPE ( 'NONE', 'NONE',  #8728 ) ;
#6246 = CARTESIAN_POINT ( 'NONE',  ( -31.62280801364509486, -40.25948930238543966, 12.39794155511765794 ) ) ;
#6247 = CARTESIAN_POINT ( 'NONE',  ( 4.566987299999998307, -43.10829192115428299, -98.19999999890751496 ) ) ;
#6248 = DIRECTION ( 'NONE',  ( 0.7061138087190598212, -0.05297714858780431385, -0.7061138087190823587 ) ) ;
#6249 = DIRECTION ( 'NONE',  ( -0.000000000000000000, -0.000000000000000000, -1.000000000000000000 ) ) ;
#6250 = EDGE_CURVE ( 'NONE', #6933, #5109, #431, .T. ) ;
#6251 = VERTEX_POINT ( 'NONE', #8475 ) ;
#6252 = CARTESIAN_POINT ( 'NONE',  ( -34.10713997105786888, -46.14859572486944472, -7.938018618334151455 ) ) ;
#6253 = CARTESIAN_POINT ( 'NONE',  ( -23.28248557872775137, -43.50000000000001421, 6.717514421272141156 ) ) ;
#6254 = ORIENTED_EDGE ( 'NONE', *, *, #1189, .F. ) ;
#6255 = ADVANCED_FACE ( 'NONE', ( #1106 ), #5569, .T. ) ;
#6256 = CARTESIAN_POINT ( 'NONE',  ( -23.28248557872775137, -46.50000000000000711, 6.717514421272141156 ) ) ;
#6257 = DIRECTION ( 'NONE',  ( -0.000000000000000000, 1.000000000000000000, 0.000000000000000000 ) ) ;
#6258 = CIRCLE ( 'NONE', #6949, 12.00000000000004263 ) ;
#6259 = CARTESIAN_POINT ( 'NONE',  ( 2.071067811865474173, -39.99999999999997158, -98.34999999781506119 ) ) ;
#6260 = CARTESIAN_POINT ( 'NONE',  ( -23.28248557872775137, -49.50000000000000711, 6.717514421272141156 ) ) ;
#6261 = CARTESIAN_POINT ( 'NONE',  ( 3.229347689422839895, -41.77065231057713390, -98.74999999890752633 ) ) ;
#6262 = ORIENTED_EDGE ( 'NONE', *, *, #2490, .F. ) ;
#6263 = CARTESIAN_POINT ( 'NONE',  ( -38.38706344316003793, -46.70140427513057801, -1.382017864820032083 ) ) ;
#6264 = CARTESIAN_POINT ( 'NONE',  ( -2.071067811865475061, -39.99999999999997158, -99.14300000002185698 ) ) ;
#6265 = CARTESIAN_POINT ( 'NONE',  ( -33.85891924778610473, -50.10000000000000853, 7.573555455601171715 ) ) ;
#6266 = CARTESIAN_POINT ( 'NONE',  ( 42.00000000000000711, -21.99999999999992184, 60.00000000000002842 ) ) ;
#6267 = PRODUCT_CONTEXT ( 'NONE', #1202, 'mechanical' ) ;
#6268 = CARTESIAN_POINT ( 'NONE',  ( -36.31971658582311591, -35.24999999999998579, 6.319716585823199395 ) ) ;
#6269 = CARTESIAN_POINT ( 'NONE',  ( -29.83554193206648009, -40.00000000000002132, 12.49999999999998046 ) ) ;
#6270 = DIRECTION ( 'NONE',  ( -1.000000000000000000, 0.000000000000000000, 0.000000000000000000 ) ) ;
#6271 = CARTESIAN_POINT ( 'NONE',  ( -25.68709025247441602, -33.60000000000000142, -8.464561979789547053 ) ) ;
#6272 = CARTESIAN_POINT ( 'NONE',  ( 4.000000000000003553, 4.286263797015736595E-16, -3.500000000000000000 ) ) ;
#6273 = CARTESIAN_POINT ( 'NONE',  ( -22.93678734525658314, -42.75000000000000711, -7.063212654743582064 ) ) ;
#6274 = ORIENTED_EDGE ( 'NONE', *, *, #8610, .F. ) ;
#6275 = DIRECTION ( 'NONE',  ( 0.000000000000000000, 0.5000000000000011102, 0.8660254037844379305 ) ) ;
#6276 = ORIENTED_EDGE ( 'NONE', *, *, #1937, .T. ) ;
#6277 = CARTESIAN_POINT ( 'NONE',  ( -38.81868038277247734, -39.54859572486944330, 1.453139578080855365 ) ) ;
#6278 = AXIS2_PLACEMENT_3D ( 'NONE', #247, #7563, #2114 ) ;
#6279 = CARTESIAN_POINT ( 'NONE',  ( -20.13408869516453947, -31.05000000000000782, -1.562606840307983136 ) ) ;
#6280 = CARTESIAN_POINT ( 'NONE',  ( -31.61762450863942320, -48.95140427513057091, 9.857197362228843573 ) ) ;
#6281 = EDGE_CURVE ( 'NONE', #923, #4984, #878, .T. ) ;
#6282 = CARTESIAN_POINT ( 'NONE',  ( 1.891708078845682595, -40.43301269999998482, -95.49999999890754054 ) ) ;
#6283 = DIRECTION ( 'NONE',  ( -0.000000000000000000, -0.000000000000000000, -1.000000000000000000 ) ) ;
#6284 = CARTESIAN_POINT ( 'NONE',  ( 3.229347689422839895, -41.77065231057713390, -98.14999999890751781 ) ) ;
#6285 = CARTESIAN_POINT ( 'NONE',  ( 5.000000000000000888, -42.92893218813449607, -95.34999999999999432 ) ) ;
#6286 = DIRECTION ( 'NONE',  ( -0.000000000000000000, 1.000000000000000000, -0.000000000000000000 ) ) ;
#6287 =( LENGTH_UNIT ( ) NAMED_UNIT ( * ) SI_UNIT ( .MILLI., .METRE. ) );
#6288 = VERTEX_POINT ( 'NONE', #5547 ) ;
#6289 = CARTESIAN_POINT ( 'NONE',  ( -31.38201786482021305, -43.29859572486943620, -8.387063443159975762 ) ) ;
#6290 = CARTESIAN_POINT ( 'NONE',  ( -22.93678734525658314, -39.74999999999999289, -7.063212654743582952 ) ) ;
#6291 = ORIENTED_EDGE ( 'NONE', *, *, #4407, .T. ) ;
#6292 = CARTESIAN_POINT ( 'NONE',  ( -38.90016716647221529, -50.84999999999999432, -4.534861676072185155 ) ) ;
#6293 = LINE ( 'NONE', #2871, #7140 ) ;
#6294 = CARTESIAN_POINT ( 'NONE',  ( 2.000000000000000000, 0.000000000000000000, 0.000000000000000000 ) ) ;
#6295 = AXIS2_PLACEMENT_3D ( 'NONE', #1612, #7602, #8322 ) ;
#6296 = CARTESIAN_POINT ( 'NONE',  ( -4.999999999999997335, -47.07106781186546129, -98.04999999781504982 ) ) ;
#6297 = CARTESIAN_POINT ( 'NONE',  ( -31.56260684030781505, -49.95000000000000995, 9.865911304835510265 ) ) ;
#6298 = AXIS2_PLACEMENT_3D ( 'NONE', #8695, #4558, #5882 ) ;
#6299 = CARTESIAN_POINT ( 'NONE',  ( 4.566987299999998307, -43.10829192115428299, -97.99999999890754054 ) ) ;
#6300 = EDGE_CURVE ( 'NONE', #6952, #5681, #5451, .T. ) ;
#6301 = ORIENTED_EDGE ( 'NONE', *, *, #5368, .T. ) ;
#6302 = CARTESIAN_POINT ( 'NONE',  ( -34.05750781543318340, -33.15000000000001279, -7.963307464738195840 ) ) ;
#6303 = AXIS2_PLACEMENT_3D ( 'NONE', #8462, #2424, #299 ) ;
#6304 = CARTESIAN_POINT ( 'NONE',  ( -4.999999999999998224, -42.92893218813448897, -95.04999999999999716 ) ) ;
#6305 = DIRECTION ( 'NONE',  ( 1.000000000000000000, 0.000000000000000000, 0.000000000000000000 ) ) ;
#6306 = CARTESIAN_POINT ( 'NONE',  ( 5.000000000000000000, -47.07106781186545419, -96.14999999781504414 ) ) ;
#6307 = CARTESIAN_POINT ( 'NONE',  ( -34.35889894354067309, 8.000000000000000000, 124.0000000000000000 ) ) ;
#6308 = FILL_AREA_STYLE ('',( #3587 ) ) ;
#6309 = CARTESIAN_POINT ( 'NONE',  ( -22.03669253526174998, -37.35000000000000853, 4.057507815433014642 ) ) ;
#6310 = EDGE_CURVE ( 'NONE', #7760, #8009, #4260, .T. ) ;
#6311 = FACE_OUTER_BOUND ( 'NONE', #3922, .T. ) ;
#6312 = LINE ( 'NONE', #3630, #3798 ) ;
#6313 = CARTESIAN_POINT ( 'NONE',  ( -25.68709025247441602, -36.60000000000000853, -8.464561979789547053 ) ) ;
#6314 = DIRECTION ( 'NONE',  ( 1.000000000000000000, 0.000000000000000000, 0.000000000000000000 ) ) ;
#6315 = CARTESIAN_POINT ( 'NONE',  ( -23.28248557872775137, -40.50000000000000711, 6.717514421272141156 ) ) ;
#6316 =( NAMED_UNIT ( * ) PLANE_ANGLE_UNIT ( ) SI_UNIT ( $, .RADIAN. ) );
#6317 = EDGE_LOOP ( 'NONE', ( #7439, #1757, #2822, #6254 ) ) ;
#6318 = DIRECTION ( 'NONE',  ( 1.000000000000000000, 0.000000000000000000, -0.000000000000000000 ) ) ;
#6319 = VERTEX_POINT ( 'NONE', #5589 ) ;
#6320 = CARTESIAN_POINT ( 'NONE',  ( -28.61798213517984024, -38.79859572486943620, 8.387063443159973986 ) ) ;
#6321 = CARTESIAN_POINT ( 'NONE',  ( -20.14280263777121149, -50.04859572486944330, -1.617624508639600833 ) ) ;
#6322 = CARTESIAN_POINT ( 'NONE',  ( -20.12537475255788522, -48.05140427513057233, -1.507589171976365439 ) ) ;
#6323 = CARTESIAN_POINT ( 'NONE',  ( -3.229347689422840784, -41.77065231057713390, -97.74999999890752633 ) ) ;
#6324 = CARTESIAN_POINT ( 'NONE',  ( -3.229347689422840784, -41.77065231057713390, -97.94999999890751496 ) ) ;
#6325 = DIRECTION ( 'NONE',  ( 1.000000000000000000, 0.000000000000000000, 0.000000000000000000 ) ) ;
#6326 = CARTESIAN_POINT ( 'NONE',  ( -1.891708078845683483, -49.56698729999997255, -96.09999999890750644 ) ) ;
#6327 = PLANE ( 'NONE',  #7894 ) ;
#6328 = ORIENTED_EDGE ( 'NONE', *, *, #2086, .T. ) ;
#6329 = EDGE_CURVE ( 'NONE', #3439, #7760, #216, .T. ) ;
#6330 = CARTESIAN_POINT ( 'NONE',  ( -21.18131961722757595, -44.04859572486944330, -1.453139578080854699 ) ) ;
#6331 = CARTESIAN_POINT ( 'NONE',  ( -21.09983283352784156, -40.35000000000000142, 4.534861676072186043 ) ) ;
#6332 = APPLICATION_CONTEXT ( 'automotive_design' ) ;
#6333 = ORIENTED_EDGE ( 'NONE', *, *, #4976, .T. ) ;
#6334 = CARTESIAN_POINT ( 'NONE',  ( -34.31290974752564438, -44.10000000000000853, 8.464561979789547053 ) ) ;
#6335 = AXIS2_PLACEMENT_3D ( 'NONE', #4032, #7953, #6578 ) ;
#6336 = DIRECTION ( 'NONE',  ( 1.000000000000000000, 0.000000000000000000, 0.000000000000000000 ) ) ;
#6337 = LINE ( 'NONE', #2253, #4018 ) ;
#6338 = CARTESIAN_POINT ( 'NONE',  ( 2.071067811865477282, -49.99999999999996447, -98.64999999781504414 ) ) ;
#6339 = DIRECTION ( 'NONE',  ( 0.000000000000000000, 0.000000000000000000, 1.000000000000000000 ) ) ;
#6340 = CARTESIAN_POINT ( 'NONE',  ( 4.999999999999998224, -44.99999999999997158, -97.79999999999999716 ) ) ;
#6341 = EDGE_CURVE ( 'NONE', #4956, #7944, #6782, .T. ) ;
#6342 = EDGE_LOOP ( 'NONE', ( #1183, #4788, #8708, #4412 ) ) ;
#6343 = PRODUCT_DEFINITION_SHAPE ( 'NONE', 'NONE',  #5889 ) ;
#6344 = CARTESIAN_POINT ( 'NONE',  ( -31.39812190974910422, -34.95000000000000995, 8.827394325379140483 ) ) ;
#6345 = CARTESIAN_POINT ( 'NONE',  ( -4.999999999999998224, -44.99999999999997158, -98.19300000002183992 ) ) ;
#6346 = CARTESIAN_POINT ( 'NONE',  ( 1.891708078845682595, -40.43301269999998482, -95.49999999890754054 ) ) ;
#6347 = CARTESIAN_POINT ( 'NONE',  ( -3.061616997868382155E-16, -39.99999999999997158, -96.69999999781504130 ) ) ;
#6348 = FACE_OUTER_BOUND ( 'NONE', #4428, .T. ) ;
#6349 = ADVANCED_FACE ( 'NONE', ( #2168 ), #6172, .T. ) ;
#6350 = CONTEXT_DEPENDENT_SHAPE_REPRESENTATION ( #1541, #4349 ) ;
#6351 = CARTESIAN_POINT ( 'NONE',  ( -41.99999999999985789, 0.000000000000000000, -41.35000000000000142 ) ) ;
#6352 = CARTESIAN_POINT ( 'NONE',  ( -23.98959235991431171, -34.50000000000000000, 6.010407640085604797 ) ) ;
#6353 = AXIS2_PLACEMENT_3D ( 'NONE', #3367, #8651, #4682 ) ;
#6354 = CARTESIAN_POINT ( 'NONE',  ( 30.00000000000000000, -49.99999999999997158, -1.102182119232617753E-14 ) ) ;
#6355 = CARTESIAN_POINT ( 'NONE',  ( -23.28248557872775137, -37.50000000000000711, 6.717514421272141156 ) ) ;
#6356 = FACE_OUTER_BOUND ( 'NONE', #4367, .T. ) ;
#6357 = CARTESIAN_POINT ( 'NONE',  ( -31.56260684030781505, -43.95000000000000284, 9.865911304835508489 ) ) ;
#6358 = CIRCLE ( 'NONE', #2567, 1.000000000000000888 ) ;
#6359 = ORIENTED_EDGE ( 'NONE', *, *, #8077, .T. ) ;
#6360 = ORIENTED_EDGE ( 'NONE', *, *, #2565, .T. ) ;
#6361 = CARTESIAN_POINT ( 'NONE',  ( -26.18828373723858149, -37.59859572486943335, -7.597606577763319713 ) ) ;
#6362 = CARTESIAN_POINT ( 'NONE',  ( -21.07454398712378918, -47.34859572486942625, 4.485229520447505003 ) ) ;
#6363 = AXIS2_PLACEMENT_3D ( 'NONE', #874, #831, #4854 ) ;
#6364 = CARTESIAN_POINT ( 'NONE',  ( -28.56619749409589204, -48.80140427513057233, 9.391326687552490782 ) ) ;
#6365 = CARTESIAN_POINT ( 'NONE',  ( -33.35889894354067309, -8.999999999999998224, 124.0000000000000000 ) ) ;
#6366 = SPHERICAL_SURFACE ( 'NONE', #2505, 1.000000000000000000 ) ;
#6367 = CARTESIAN_POINT ( 'NONE',  ( -25.68709025247441602, -33.60000000000000142, -8.464561979789547053 ) ) ;
#6368 = VECTOR ( 'NONE', #4618, 1000.000000000000000 ) ;
#6369 = CARTESIAN_POINT ( 'NONE',  ( -4.566987299999997418, -46.89170807884566727, -99.39999999890751781 ) ) ;
#6370 = CARTESIAN_POINT ( 'NONE',  ( 39.99999999999996447, 1.102182119232617753E-14, 60.00000000000002842 ) ) ;
#6371 = CARTESIAN_POINT ( 'NONE',  ( 8.389419568037416259E-16, -49.56698729999997255, -96.84999999890752065 ) ) ;
#6372 = DIRECTION ( 'NONE',  ( -0.000000000000000000, -0.000000000000000000, -1.000000000000000000 ) ) ;
#6373 = ORIENTED_EDGE ( 'NONE', *, *, #5756, .T. ) ;
#6374 = CARTESIAN_POINT ( 'NONE',  ( -22.45049566656107842, -43.89859572486944472, -3.906122232810846917 ) ) ;
#6375 = CARTESIAN_POINT ( 'NONE',  ( -21.09983283352784156, -43.35000000000000853, 4.534861676072186043 ) ) ;
#6376 = EDGE_CURVE ( 'NONE', #3394, #1209, #6124, .T. ) ;
#6377 = ORIENTED_EDGE ( 'NONE', *, *, #7702, .T. ) ;
#6378 = CARTESIAN_POINT ( 'NONE',  ( -23.31994607974211675, -39.50140427513058228, 6.754974922286503869 ) ) ;
#6379 = CARTESIAN_POINT ( 'NONE',  ( -34.49011023859264924, -47.22366675470355091, 11.66649199791333125 ) ) ;
#6380 = DIRECTION ( 'NONE',  ( 0.000000000000000000, 0.000000000000000000, 1.000000000000000000 ) ) ;
#6381 = DIRECTION ( 'NONE',  ( 1.000000000000000000, 0.000000000000000000, 0.000000000000000000 ) ) ;
#6382 = EDGE_CURVE ( 'NONE', #2302, #8507, #3561, .T. ) ;
#6383 = CARTESIAN_POINT ( 'NONE',  ( 29.99999999999997158, 1.102182119232617753E-14, 60.00000000000002842 ) ) ;
#6384 = CARTESIAN_POINT ( 'NONE',  ( 4.999999999999998224, -44.99999999999997158, -97.00000000000000000 ) ) ;
#6385 = VERTEX_POINT ( 'NONE', #2212 ) ;
#6386 = CARTESIAN_POINT ( 'NONE',  ( -37.96330746473829976, -35.84999999999998721, -4.057507815433013754 ) ) ;
#6387 = PRODUCT_DEFINITION_SHAPE ( 'NONE', 'NONE',  #8732 ) ;
#6388 = EDGE_CURVE ( 'NONE', #876, #6150, #6140, .T. ) ;
#6389 = VERTEX_POINT ( 'NONE', #4274 ) ;
#6390 = CARTESIAN_POINT ( 'NONE',  ( -2.071067811865475505, -49.99999999999996447, -98.04999999999999716 ) ) ;
#6391 = CARTESIAN_POINT ( 'NONE',  ( 3.535533905932737309, -48.53553390593270933, -97.79999999781504982 ) ) ;
#6392 = CARTESIAN_POINT ( 'NONE',  ( 0.000000000000000000, -0.8865213383406692627, 1.535500000000001641 ) ) ;
#6393 = ITEM_DEFINED_TRANSFORMATION ( 'NONE', 'NONE', #2995,  #2554 ) ;
#6394 = EDGE_CURVE ( 'NONE', #7878, #6586, #4677, .T. ) ;
#6395 = FACE_OUTER_BOUND ( 'NONE', #6317, .T. ) ;
#6396 = CARTESIAN_POINT ( 'NONE',  ( -31.39812190974910422, -43.95000000000000284, 8.827394325379140483 ) ) ;
#6397 = DIRECTION ( 'NONE',  ( 0.000000000000000000, 1.224646799147353207E-16, 1.000000000000000000 ) ) ;
#6398 = EDGE_CURVE ( 'NONE', #8668, #4874, #2006, .T. ) ;
#6399 = DIRECTION ( 'NONE',  ( 1.000000000000000000, 0.000000000000000000, 0.000000000000000000 ) ) ;
#6400 = DIRECTION ( 'NONE',  ( 1.000000000000000000, 0.000000000000000000, 0.000000000000000000 ) ) ;
#6401 = CARTESIAN_POINT ( 'NONE',  ( -39.38303923565386100, -38.70000000000000284, -1.486127417882099788 ) ) ;
#6402 = DIRECTION ( 'NONE',  ( -0.000000000000000000, -0.000000000000000000, -1.000000000000000000 ) ) ;
#6403 = CARTESIAN_POINT ( 'NONE',  ( -38.90016716647221529, -41.85000000000000142, -4.534861676072185155 ) ) ;
#6404 = EDGE_CURVE ( 'NONE', #864, #8551, #4400, .T. ) ;
#6405 = ORIENTED_EDGE ( 'NONE', *, *, #8610, .T. ) ;
#6406 = CARTESIAN_POINT ( 'NONE',  ( -37.98859631114233792, -51.84859572486944757, -4.007875659808334490 ) ) ;
#6407 = CARTESIAN_POINT ( 'NONE',  ( -22.93678734525658314, -30.75000000000000000, -7.063212654743582952 ) ) ;
#6408 = CARTESIAN_POINT ( 'NONE',  ( -38.87487832006816291, -49.85140427513058370, -4.584493831696867971 ) ) ;
#6409 = DIRECTION ( 'NONE',  ( -0.000000000000000000, -0.000000000000000000, -1.000000000000000000 ) ) ;
#6410 = DIRECTION ( 'NONE',  ( -0.000000000000000000, 1.000000000000000000, 0.000000000000000000 ) ) ;
#6411 = CARTESIAN_POINT ( 'NONE',  ( -20.13408869516453947, -40.05000000000001137, -1.562606840307983136 ) ) ;
#6412 = DIRECTION ( 'NONE',  ( 0.7071067811865556774, 0.000000000000000000, 0.7071067811865392461 ) ) ;
#6413 = DIRECTION ( 'NONE',  ( -0.000000000000000000, 1.000000000000000000, -0.000000000000000000 ) ) ;
#6414 = CARTESIAN_POINT ( 'NONE',  ( 3.229347689422839895, -41.77065231057713390, -98.14999999890751781 ) ) ;
#6415 = CARTESIAN_POINT ( 'NONE',  ( -3.061616997868382155E-16, -39.99999999999997158, -100.6999999978150555 ) ) ;
#6416 = VERTEX_POINT ( 'NONE', #1625 ) ;
#6417 = CARTESIAN_POINT ( 'NONE',  ( -37.54950433343896776, -39.39859572486943762, 3.906122232810848249 ) ) ;
#6418 = CARTESIAN_POINT ( 'NONE',  ( -28.43739315969223824, -48.44999999999999574, -9.865911304835512041 ) ) ;
#6419 = EDGE_CURVE ( 'NONE', #4083, #6251, #6466, .T. ) ;
#6420 = ORIENTED_EDGE ( 'NONE', *, *, #6419, .T. ) ;
#6421 = CARTESIAN_POINT ( 'NONE',  ( -22.89739904353894318, -32.75140427513057517, -7.023824353025938549 ) ) ;
#6423 = FACE_OUTER_BOUND ( 'NONE', #2393, .T. ) ;
#6422 =( BOUNDED_SURFACE ( )  B_SPLINE_SURFACE ( 1, 2, ( 
 ( #5160, #3319, #5993, #747, #7407, #4105, #1989, #5413, #1364, #7317, #5327, #2612, #6740, #2082, #5458, #2792, #2035, #2746, #2658, #6605, #8123, #4063, #700, #7273, #4722, #4676, #7364, #6783, #3930, #1233, #4767, #1272, #3452, #8685, #1903, #88, #3972, #6695, #8027, #3363, #4589, #1318, #3406, #6036, #561, #8075, #6652, #6128, #1409, #3274, #7452, #5953, #7986, #607, #4630, #4017, #8646, #656, #5279, #6084, #1945, #1998, #2700, #5369, #42, #879, #6345, #2966, #970, #8299, #132, #2260, #2306, #2130, #4811, #7579, #4942, #4151, #5597, #3581, #7007, #4280, #6215, #1540, #6828, #6264, #7622, #5505, #794, #179, #2923, #1586, #4987, #5640, #221, #3665, #6962, #1632, #8257, #8341, #927, #4858, #2878, #2831, #3621 ),
 ( #7668, #308, #3537, #6304, #3496, #835, #4325, #3010, #264, #8167, #7495, #1457, #6175, #8214, #5550, #2171, #7535, #4235, #1495, #2217, #6916, #4901, #4191, #6873, #5906, #2434, #2474, #1227, #3834, #5774, #8594, #2559, #7931, #3880, #5236, #3750, #8471, #388, #8512, #6559, #5115, #7266, #5194, #1728, #2394, #3224, #5156, #3794, #7847, #4582, #1186, #1898, #6515, #7100, #468, #512, #347, #3055, #5821, #3182, #5070, #5862, #1813, #6390, #2518, #4454, #4494, #7761, #7182, #8554, #6435, #4413, #7139, #1141, #7890, #5732, #8430, #1857, #1057, #3094, #4538, #7223, #7807, #1773, #1101, #6473, #426, #3141, #4056, #694, #5321, #3924, #741, #648, #7445, #4669, #3357, #2785, #6032, #6643, #8640, #1266, #2606, #4099, #6776 ),
 ( #4804, #600, #2652, #5988, #79, #4625, #5274, #7309, #8021, #1981, #5450, #8162, #3966, #1403, #7357, #6735, #2122, #5226, #3266, #3400, #5363, #7487, #3446, #3314, #8116, #6599, #7978, #2694, #6077, #1940, #8066, #8679, #1311, #35, #2029, #4011, #4717, #6690, #7401, #1356, #2738, #5946, #554, #5407, #2074, #4761, #6123, #2299, #8294, #6296, #920, #3658, #8333, #5678, #3616, #6259, #7530, #2341, #4186, #174, #3532, #6338, #2167, #2255, #2960, #6209, #1452, #873, #1624, #7573, #6956, #7663, #1580, #3004, #4145, #4981, #4316, #5022, #5546, #7615, #6171, #2873, #963, #8382, #4933, #7000, #6823, #5587, #4273, #787, #4895, #2826, #1490, #3575, #301, #4228, #215, #8251, #5498, #3489, #256, #5634, #127, #2210, #8208 ) ),
 .UNSPECIFIED., .F., .F., .T. ) 
 B_SPLINE_SURFACE_WITH_KNOTS ( ( 2, 1, 2 ),
 ( 3, 2, 2, 2, 2, 2, 2, 2, 2, 2, 2, 2, 2, 2, 2, 2, 2, 2, 2, 2, 2, 2, 2, 2, 2, 2, 2, 2, 2, 2, 2, 2, 2, 2, 2, 2, 2, 2, 2, 2, 2, 2, 2, 2, 2, 2, 2, 2, 2, 2, 2, 2, 3 ),
 ( -0.01000000000000000021, 0.000000000000000000, 1.000000000000000000 ),
 ( -0.008928571428571429811, 0.000000000000000000, 0.01785714285714285615, 0.03571428571428571230, 0.05357142857142856845, 0.07142857142857142461, 0.08928571428571428770, 0.1071428571428571369, 0.1250000000000000000, 0.1428571428571428492, 0.1607142857142857262, 0.1785714285714285754, 0.1964285714285714246, 0.2142857142857142738, 0.2321428571428571508, 0.2500000000000000000, 0.2678571428571428492, 0.2857142857142856984, 0.3035714285714285476, 0.3214285714285714524, 0.3392857142857143016, 0.3571428571428571508, 0.3750000000000000000, 0.3928571428571428492, 0.4107142857142856984, 0.4285714285714285476, 0.4464285714285714524, 0.4642857142857143016, 0.4821428571428571508, 0.5000000000000000000, 0.5178571428571429047, 0.5357142857142856984, 0.5535714285714286031, 0.5714285714285713969, 0.5892857142857143016, 0.6071428571428570953, 0.6250000000000000000, 0.6428571428571429047, 0.6607142857142856984, 0.6785714285714286031, 0.6964285714285713969, 0.7142857142857143016, 0.7321428571428570953, 0.7500000000000000000, 0.7678571428571429047, 0.7857142857142856984, 0.8035714285714286031, 0.8214285714285713969, 0.8392857142857143016, 0.8571428571428570953, 0.8750000000000000000, 0.8928571428571429047, 0.9018750000000000933 ),
 .UNSPECIFIED. ) 
 GEOMETRIC_REPRESENTATION_ITEM ( )  RATIONAL_B_SPLINE_SURFACE ( (
 ( 1.000000000000000000, 1.000000000000000000, 1.000000000000000000, 0.9238795325112867385, 1.000000000000000000, 0.9238795325112867385, 1.000000000000000000, 0.9238795325112867385, 1.000000000000000000, 0.9238795325112867385, 1.000000000000000000, 0.9238795325112867385, 1.000000000000000000, 0.9238795325112867385, 1.000000000000000000, 0.9238795325112867385, 1.000000000000000000, 0.9238795325112867385, 1.000000000000000000, 0.9238795325112867385, 1.000000000000000000, 0.9238795325112867385, 1.000000000000000000, 0.9238795325112867385, 1.000000000000000000, 0.9238795325112867385, 1.000000000000000000, 0.9238795325112867385, 1.000000000000000000, 0.9238795325112867385, 1.000000000000000000, 0.9238795325112867385, 1.000000000000000000, 0.9238795325112867385, 1.000000000000000000, 0.9238795325112867385, 1.000000000000000000, 0.9238795325112867385, 1.000000000000000000, 0.9238795325112867385, 1.000000000000000000, 0.9238795325112867385, 1.000000000000000000, 0.9238795325112867385, 1.000000000000000000, 0.9238795325112867385, 1.000000000000000000, 0.9238795325112867385, 1.000000000000000000, 0.9238795325112867385, 1.000000000000000000, 0.9238795325112867385, 1.000000000000000000, 0.9238795325112867385, 1.000000000000000000, 0.9238795325112867385, 1.000000000000000000, 0.9238795325112867385, 1.000000000000000000, 0.9238795325112867385, 1.000000000000000000, 0.9238795325112867385, 1.000000000000000000, 0.9238795325112867385, 1.000000000000000000, 0.9238795325112867385, 1.000000000000000000, 0.9238795325112867385, 1.000000000000000000, 0.9238795325112867385, 1.000000000000000000, 0.9238795325112867385, 1.000000000000000000, 0.9238795325112867385, 1.000000000000000000, 0.9238795325112867385, 1.000000000000000000, 0.9238795325112867385, 1.000000000000000000, 0.9238795325112867385, 1.000000000000000000, 0.9238795325112867385, 1.000000000000000000, 0.9238795325112867385, 1.000000000000000000, 0.9238795325112867385, 1.000000000000000000, 0.9238795325112867385, 1.000000000000000000, 0.9238795325112867385, 1.000000000000000000, 0.9238795325112867385, 1.000000000000000000, 0.9238795325112867385, 1.000000000000000000, 0.9238795325112867385, 1.000000000000000000, 0.9238795325112867385, 1.000000000000000000, 0.9238795325112867385, 1.000000000000000000, 0.9238795325112867385, 1.000000000000000000, 1.000000000000000000, 1.000000000000000000),
 ( 1.000000000000000000, 1.000000000000000000, 1.000000000000000000, 0.9238795325112867385, 1.000000000000000000, 0.9238795325112867385, 1.000000000000000000, 0.9238795325112867385, 1.000000000000000000, 0.9238795325112867385, 1.000000000000000000, 0.9238795325112867385, 1.000000000000000000, 0.9238795325112867385, 1.000000000000000000, 0.9238795325112867385, 1.000000000000000000, 0.9238795325112867385, 1.000000000000000000, 0.9238795325112867385, 1.000000000000000000, 0.9238795325112867385, 1.000000000000000000, 0.9238795325112867385, 1.000000000000000000, 0.9238795325112867385, 1.000000000000000000, 0.9238795325112867385, 1.000000000000000000, 0.9238795325112867385, 1.000000000000000000, 0.9238795325112867385, 1.000000000000000000, 0.9238795325112867385, 1.000000000000000000, 0.9238795325112867385, 1.000000000000000000, 0.9238795325112867385, 1.000000000000000000, 0.9238795325112867385, 1.000000000000000000, 0.9238795325112867385, 1.000000000000000000, 0.9238795325112867385, 1.000000000000000000, 0.9238795325112867385, 1.000000000000000000, 0.9238795325112867385, 1.000000000000000000, 0.9238795325112867385, 1.000000000000000000, 0.9238795325112867385, 1.000000000000000000, 0.9238795325112867385, 1.000000000000000000, 0.9238795325112867385, 1.000000000000000000, 0.9238795325112867385, 1.000000000000000000, 0.9238795325112867385, 1.000000000000000000, 0.9238795325112867385, 1.000000000000000000, 0.9238795325112867385, 1.000000000000000000, 0.9238795325112867385, 1.000000000000000000, 0.9238795325112867385, 1.000000000000000000, 0.9238795325112867385, 1.000000000000000000, 0.9238795325112867385, 1.000000000000000000, 0.9238795325112867385, 1.000000000000000000, 0.9238795325112867385, 1.000000000000000000, 0.9238795325112867385, 1.000000000000000000, 0.9238795325112867385, 1.000000000000000000, 0.9238795325112867385, 1.000000000000000000, 0.9238795325112867385, 1.000000000000000000, 0.9238795325112867385, 1.000000000000000000, 0.9238795325112867385, 1.000000000000000000, 0.9238795325112867385, 1.000000000000000000, 0.9238795325112867385, 1.000000000000000000, 0.9238795325112867385, 1.000000000000000000, 0.9238795325112867385, 1.000000000000000000, 0.9238795325112867385, 1.000000000000000000, 0.9238795325112867385, 1.000000000000000000, 0.9238795325112867385, 1.000000000000000000, 1.000000000000000000, 1.000000000000000000),
 ( 1.000000000000000000, 1.000000000000000000, 1.000000000000000000, 0.9238795325112867385, 1.000000000000000000, 0.9238795325112867385, 1.000000000000000000, 0.9238795325112867385, 1.000000000000000000, 0.9238795325112867385, 1.000000000000000000, 0.9238795325112867385, 1.000000000000000000, 0.9238795325112867385, 1.000000000000000000, 0.9238795325112867385, 1.000000000000000000, 0.9238795325112867385, 1.000000000000000000, 0.9238795325112867385, 1.000000000000000000, 0.9238795325112867385, 1.000000000000000000, 0.9238795325112867385, 1.000000000000000000, 0.9238795325112867385, 1.000000000000000000, 0.9238795325112867385, 1.000000000000000000, 0.9238795325112867385, 1.000000000000000000, 0.9238795325112867385, 1.000000000000000000, 0.9238795325112867385, 1.000000000000000000, 0.9238795325112867385, 1.000000000000000000, 0.9238795325112867385, 1.000000000000000000, 0.9238795325112867385, 1.000000000000000000, 0.9238795325112867385, 1.000000000000000000, 0.9238795325112867385, 1.000000000000000000, 0.9238795325112867385, 1.000000000000000000, 0.9238795325112867385, 1.000000000000000000, 0.9238795325112867385, 1.000000000000000000, 0.9238795325112867385, 1.000000000000000000, 0.9238795325112867385, 1.000000000000000000, 0.9238795325112867385, 1.000000000000000000, 0.9238795325112867385, 1.000000000000000000, 0.9238795325112867385, 1.000000000000000000, 0.9238795325112867385, 1.000000000000000000, 0.9238795325112867385, 1.000000000000000000, 0.9238795325112867385, 1.000000000000000000, 0.9238795325112867385, 1.000000000000000000, 0.9238795325112867385, 1.000000000000000000, 0.9238795325112867385, 1.000000000000000000, 0.9238795325112867385, 1.000000000000000000, 0.9238795325112867385, 1.000000000000000000, 0.9238795325112867385, 1.000000000000000000, 0.9238795325112867385, 1.000000000000000000, 0.9238795325112867385, 1.000000000000000000, 0.9238795325112867385, 1.000000000000000000, 0.9238795325112867385, 1.000000000000000000, 0.9238795325112867385, 1.000000000000000000, 0.9238795325112867385, 1.000000000000000000, 0.9238795325112867385, 1.000000000000000000, 0.9238795325112867385, 1.000000000000000000, 0.9238795325112867385, 1.000000000000000000, 0.9238795325112867385, 1.000000000000000000, 0.9238795325112867385, 1.000000000000000000, 0.9238795325112867385, 1.000000000000000000, 1.000000000000000000, 1.000000000000000000) ) ) 
 REPRESENTATION_ITEM ( '' )  SURFACE ( )  );
#6424 = DIRECTION ( 'NONE',  ( -1.000000000000000000, 0.000000000000000000, 0.000000000000000000 ) ) ;
#6425 = LINE ( 'NONE', #5187, #2152 ) ;
#6426 = AXIS2_PLACEMENT_3D ( 'NONE', #3380, #1291, #3992 ) ;
#6427 = DIRECTION ( 'NONE',  ( -1.000000000000000000, 0.000000000000000000, 0.000000000000000000 ) ) ;
#6428 = CARTESIAN_POINT ( 'NONE',  ( 2.071067811865477282, -49.99999999999996447, -95.54999999999999716 ) ) ;
#6429 = ORIENTED_EDGE ( 'NONE', *, *, #4029, .T. ) ;
#6430 = CIRCLE ( 'NONE', #1926, 12.00000000000004263 ) ;
#6431 = CARTESIAN_POINT ( 'NONE',  ( -25.94249218456686279, -37.65000000000000568, 7.963307464738195840 ) ) ;
#6432 = AXIS2_PLACEMENT_3D ( 'NONE', #7739, #3116, #4472 ) ;
#6433 = EDGE_LOOP ( 'NONE', ( #4612, #4519, #15, #1811 ) ) ;
#6434 = UNCERTAINTY_MEASURE_WITH_UNIT (LENGTH_MEASURE( 1.000000000000000082E-05 ), #6932, 'distance_accuracy_value', 'NONE');
#6435 = CARTESIAN_POINT ( 'NONE',  ( -3.061616997868382155E-16, -39.99999999999997158, -98.40000000000000568 ) ) ;
#6436 = CARTESIAN_POINT ( 'NONE',  ( -4.999999999999998224, -44.99999999999997158, -98.09999999781504698 ) ) ;
#6437 = CARTESIAN_POINT ( 'NONE',  ( -42.00000000000002132, 0.000000000000000000, -29.65000000000000213 ) ) ;
#6438 = EDGE_CURVE ( 'NONE', #5475, #999, #7777, .T. ) ;
#6439 = DIRECTION ( 'NONE',  ( 0.000000000000000000, 0.000000000000000000, 1.000000000000000000 ) ) ;
#6440 = AXIS2_PLACEMENT_3D ( 'NONE', #610, #1320, #2614 ) ;
#6441 = CYLINDRICAL_SURFACE ( 'NONE', #3605, 10.00000000000000178 ) ;
#6442 = CARTESIAN_POINT ( 'NONE',  ( 4.999999999999998224, -44.99999999999997158, -98.60000000000000853 ) ) ;
#6443 = DIRECTION ( 'NONE',  ( -1.000000000000000000, 0.000000000000000000, 0.000000000000000000 ) ) ;
#6444 = CARTESIAN_POINT ( 'NONE',  ( 2.000000000000000000, -0.8865213383406692627, 1.535500000000001641 ) ) ;
#6445 = CARTESIAN_POINT ( 'NONE',  ( -20.13408869516454303, -37.05000000000000426, -1.562606840307982692 ) ) ;
#6446 = EDGE_LOOP ( 'NONE', ( #4772, #7708, #6190 ) ) ;
#6447 = CARTESIAN_POINT ( 'NONE',  ( -36.04786814110010340, -45.99859572486943904, -5.972947139071243861 ) ) ;
#6448 = CARTESIAN_POINT ( 'NONE',  ( -28.43739315969223824, -36.45000000000000284, -9.865911304835512041 ) ) ;
#6449 = CARTESIAN_POINT ( 'NONE',  ( -26.09387776718931917, -38.60140427513057659, -7.549504333439021941 ) ) ;
#6450 = DIRECTION ( 'NONE',  ( -0.000000000000000000, -0.000000000000000000, 1.000000000000000000 ) ) ;
#6451 = CARTESIAN_POINT ( 'NONE',  ( -2.796473189345805913E-16, -40.43301269999997061, -100.2499999989075263 ) ) ;
#6452 = CARTESIAN_POINT ( 'NONE',  ( -25.68709025247441602, -36.60000000000000853, -8.464561979789547053 ) ) ;
#6453 = FACE_OUTER_BOUND ( 'NONE', #3571, .T. ) ;
#6454 = DIRECTION ( 'NONE',  ( -1.000000000000000000, -0.000000000000000000, -0.000000000000000000 ) ) ;
#6455 = CARTESIAN_POINT ( 'NONE',  ( -4.566987299999997418, -46.89170807884566727, -96.19999999890751496 ) ) ;
#6456 = DIRECTION ( 'NONE',  ( 0.000000000000000000, 0.000000000000000000, -1.000000000000000000 ) ) ;
#6457 = ORIENTED_EDGE ( 'NONE', *, *, #1924, .T. ) ;
#6458 = DIRECTION ( 'NONE',  ( -0.000000000000000000, 1.000000000000000000, -0.000000000000000000 ) ) ;
#6459 = CARTESIAN_POINT ( 'NONE',  ( -34.10713997105786888, -49.14859572486945183, -7.938018618334151455 ) ) ;
#6460 = CARTESIAN_POINT ( 'NONE',  ( -22.89739904353894318, -32.75140427513057517, -7.023824353025938549 ) ) ;
#6461 = ORIENTED_EDGE ( 'NONE', *, *, #5588, .F. ) ;
#6462 = CARTESIAN_POINT ( 'NONE',  ( -20.12537475255788522, -39.05140427513057944, -1.507589171976365439 ) ) ;
#6463 = CARTESIAN_POINT ( 'NONE',  ( -3.061616997868382155E-16, -39.99999999999997158, -96.69999999781504130 ) ) ;
#6464 = PLANE ( 'NONE',  #8491 ) ;
#6465 = CARTESIAN_POINT ( 'NONE',  ( 3.535533905932736420, -41.46446609406723383, -97.59999999781504698 ) ) ;
#6466 = LINE ( 'NONE', #3005, #2858 ) ;
#6467 = CARTESIAN_POINT ( 'NONE',  ( 3.535533905932737309, -48.53553390593270933, -97.10000000000000853 ) ) ;
#6468 = EDGE_LOOP ( 'NONE', ( #2507, #3650, #7557 ) ) ;
#6469 = CARTESIAN_POINT ( 'NONE',  ( -36.01040764008574513, -36.00000000000000711, -6.010407640085605685 ) ) ;
#6470 = AXIS2_PLACEMENT_3D ( 'NONE', #3077, #3858, #5051 ) ;
#6471 = SHAPE_REPRESENTATION ( 'position indicator', ( #2554 ), #564 ) ;
#6472 = ORIENTED_EDGE ( 'NONE', *, *, #250, .F. ) ;
#6473 = CARTESIAN_POINT ( 'NONE',  ( -2.071067811865475061, -39.99999999999997158, -99.14999999999999147 ) ) ;
#6474 = AXIS2_PLACEMENT_3D ( 'NONE', #576, #670, #3291 ) ;
#6475 = CARTESIAN_POINT ( 'NONE',  ( -2.449416140927843877, -49.39737961008592038, -100.0005770061920884 ) ) ;
#6476 = DIRECTION ( 'NONE',  ( 0.000000000000000000, 0.000000000000000000, 1.000000000000000000 ) ) ;
#6477 = CYLINDRICAL_SURFACE ( 'NONE', #7074, 4.999999999999998224 ) ;
#6478 = AXIS2_PLACEMENT_3D ( 'NONE', #82, #2789, #8025 ) ;
#6479 = DIRECTION ( 'NONE',  ( -0.000000000000000000, 0.000000000000000000, 1.000000000000000000 ) ) ;
#6480 = LINE ( 'NONE', #7815, #1686 ) ;
#6481 = DIRECTION ( 'NONE',  ( -1.000000000000000000, 0.000000000000000000, 0.000000000000000000 ) ) ;
#6482 = MECHANICAL_DESIGN_GEOMETRIC_PRESENTATION_REPRESENTATION (  '', ( #302 ), #5357 ) ;
#6483 = PLANE ( 'NONE',  #3147 ) ;
#6484 = EDGE_CURVE ( 'NONE', #999, #5475, #2715, .T. ) ;
#6485 = PRESENTATION_STYLE_ASSIGNMENT (( #3027 ) ) ;
#6486 = ORIENTED_EDGE ( 'NONE', *, *, #6490, .T. ) ;
#6487 = CARTESIAN_POINT ( 'NONE',  ( -21.55948914237271907, -31.89859572486943762, -4.360112732550413206 ) ) ;
#6488 = CARTESIAN_POINT ( 'NONE',  ( -22.93678734525658314, -36.75000000000000711, -7.063212654743582952 ) ) ;
#6489 = CARTESIAN_POINT ( 'NONE',  ( -34.00787565980851213, -35.15140427513058086, -7.988596311142238449 ) ) ;
#6490 = EDGE_CURVE ( 'NONE', #6385, #6859, #32, .T. ) ;
#6491 = CARTESIAN_POINT ( 'NONE',  ( -4.566987299999997418, -46.89170807884566017, -99.99999999890754054 ) ) ;
#6492 = DIRECTION ( 'NONE',  ( -0.000000000000000000, 1.000000000000000000, -0.000000000000000000 ) ) ;
#6493 = CARTESIAN_POINT ( 'NONE',  ( -25.73429323749904185, -37.59859572486943335, -8.488613101951701267 ) ) ;
#6494 = CARTESIAN_POINT ( 'NONE',  ( -39.86591130483550671, -32.55000000000000426, 1.562606840307984468 ) ) ;
#6495 = CARTESIAN_POINT ( 'NONE',  ( 8.389419568037416259E-16, -49.56698729999997255, -100.0499999989075093 ) ) ;
#6496 = CARTESIAN_POINT ( 'NONE',  ( 42.00000000000000711, 21.99999999999992184, 80.00000000000002842 ) ) ;
#6497 = CARTESIAN_POINT ( 'NONE',  ( -3.229347689422839451, -48.22934768942280925, -96.94999999890751496 ) ) ;
#6498 = EDGE_LOOP ( 'NONE', ( #1537, #450, #7613, #2994 ) ) ;
#6499 = CARTESIAN_POINT ( 'NONE',  ( -33.81171626276147890, -48.09859572486944046, 7.597606577763319713 ) ) ;
#6500 = CARTESIAN_POINT ( 'NONE',  ( -28.56619749409589204, -30.80140427513057233, 9.391326687552490782 ) ) ;
#6501 = ADVANCED_FACE ( 'NONE', ( #1094 ), #3050, .T. ) ;
#6502 = ORIENTED_EDGE ( 'NONE', *, *, #6999, .F. ) ;
#6503 = AXIS2_PLACEMENT_3D ( 'NONE', #8434, #2397, #6439 ) ;
#6504 = CARTESIAN_POINT ( 'NONE',  ( -37.10260095646111012, -34.25140427513057517, 7.023824353025939438 ) ) ;
#6505 = FACE_OUTER_BOUND ( 'NONE', #3997, .T. ) ;
#6506 = LINE ( 'NONE', #1177, #1735 ) ;
#6507 = CYLINDRICAL_SURFACE ( 'NONE', #7490, 11.99999999999979217 ) ;
#6508 = CARTESIAN_POINT ( 'NONE',  ( 42.00000000000000711, 47.00857997860455129, 21.99999999999992184 ) ) ;
#6509 = CARTESIAN_POINT ( 'NONE',  ( -4.999999999999998224, -44.99999999999997158, -97.40000000000000568 ) ) ;
#6510 = EDGE_LOOP ( 'NONE', ( #5392, #983 ) ) ;
#6511 = AXIS2_PLACEMENT_3D ( 'NONE', #3366, #2750, #3498 ) ;
#6512 = CARTESIAN_POINT ( 'NONE',  ( -23.98959235991431171, -43.50000000000001421, 6.010407640085604797 ) ) ;
#6513 = EDGE_CURVE ( 'NONE', #8204, #5819, #7713, .T. ) ;
#6514 = ORIENTED_EDGE ( 'NONE', *, *, #6158, .F. ) ;
#6515 = CARTESIAN_POINT ( 'NONE',  ( -3.535533905932736864, -41.46446609406723383, -97.50000000000000000 ) ) ;
#6516 = AXIS2_PLACEMENT_3D ( 'NONE', #2196, #6985, #3688 ) ;
#6517 = CARTESIAN_POINT ( 'NONE',  ( 0.3202549665280822189, -49.99785177082193854, -100.0005802109309059 ) ) ;
#6518 = CARTESIAN_POINT ( 'NONE',  ( -22.06198138166579170, -33.35140427513057659, 4.107139971057695682 ) ) ;
#6519 = LINE ( 'NONE', #4373, #2154 ) ;
#6520 = ADVANCED_FACE ( 'NONE', ( #7173 ), #3424, .F. ) ;
#6521 = VECTOR ( 'NONE', #6815, 1000.000000000000000 ) ;
#6522 = EDGE_CURVE ( 'NONE', #4594, #1795, #4405, .T. ) ;
#6523 = DIRECTION ( 'NONE',  ( -1.000000000000000000, 0.000000000000000000, 0.000000000000000000 ) ) ;
#6524 = CARTESIAN_POINT ( 'NONE',  ( -33.85891924778610473, -35.10000000000000853, 7.573555455601171715 ) ) ;
#6525 = CIRCLE ( 'NONE', #6091, 2.000000000000000888 ) ;
#6526 = CARTESIAN_POINT ( 'NONE',  ( 0.000000000000000000, -44.99999999999997158, -95.00000000000000000 ) ) ;
#6527 = CARTESIAN_POINT ( 'NONE',  ( -23.28248557872775137, -46.50000000000000711, 6.717514421272141156 ) ) ;
#6528 = CARTESIAN_POINT ( 'NONE',  ( 30.00000000000002842, 37.32500000000002416, 3.159706489353922981E-15 ) ) ;
#6529 = VERTEX_POINT ( 'NONE', #1134 ) ;
#6530 = CARTESIAN_POINT ( 'NONE',  ( -31.38201786482021305, -46.29859572486944330, -8.387063443159975762 ) ) ;
#6531 = CARTESIAN_POINT ( 'NONE',  ( -34.31290974752564438, -35.10000000000000853, 8.464561979789547053 ) ) ;
#6532 = CARTESIAN_POINT ( 'NONE',  ( -31.45313957808072303, -39.95140427513058512, 8.818680382772479120 ) ) ;
#6533 = CARTESIAN_POINT ( 'NONE',  ( 4.566987299999998307, -43.10829192115428299, -98.79999999890750928 ) ) ;
#6534 = DIRECTION ( 'NONE',  ( -0.000000000000000000, -0.000000000000000000, 1.000000000000000000 ) ) ;
#6535 = CARTESIAN_POINT ( 'NONE',  ( -28.46154767013959486, -35.79859572486943620, 9.374751783755112200 ) ) ;
#6536 = CARTESIAN_POINT ( 'NONE',  ( -23.28248557872775137, -34.50000000000000000, 6.717514421272141156 ) ) ;
#6537 = CARTESIAN_POINT ( 'NONE',  ( -4.566987299999998307, -44.99999999999997158, -100.2499999989075121 ) ) ;
#6538 = CARTESIAN_POINT ( 'NONE',  ( -40.00000000000002842, 1.224646799147353256E-15, -45.00000000000000000 ) ) ;
#6539 = CARTESIAN_POINT ( 'NONE',  ( 4.566987299999998307, -43.10829192115428299, -96.39999999890753202 ) ) ;
#6540 = ORIENTED_EDGE ( 'NONE', *, *, #5387, .F. ) ;
#6541 = DIRECTION ( 'NONE',  ( 0.000000000000000000, 0.000000000000000000, -1.000000000000000000 ) ) ;
#6542 = CARTESIAN_POINT ( 'NONE',  ( -20.14280263777121149, -32.04859572486944330, -1.617624508639600833 ) ) ;
#6543 = CARTESIAN_POINT ( 'NONE',  ( -37.10260095646111012, -31.25140427513058228, 7.023824353025939438 ) ) ;
#6544 = VERTEX_POINT ( 'NONE', #7046 ) ;
#6545 = ORIENTED_EDGE ( 'NONE', *, *, #7251, .T. ) ;
#6546 = CARTESIAN_POINT ( 'NONE',  ( -31.43380250590416125, -38.30140427513057944, -9.391326687552492558 ) ) ;
#6547 = AXIS2_PLACEMENT_3D ( 'NONE', #6549, #1716, #3130 ) ;
#6548 = CARTESIAN_POINT ( 'NONE',  ( -34.73327931856048423, -46.61962928414794760, 11.56930355017053280 ) ) ;
#6549 = CARTESIAN_POINT ( 'NONE',  ( -41.99999999999996447, 60.00000000000002842, 22.00000000000000000 ) ) ;
#6550 = CARTESIAN_POINT ( 'NONE',  ( 50.00000000000002842, 60.00000000000002842, 30.00000000000000000 ) ) ;
#6551 = LINE ( 'NONE', #593, #1870 ) ;
#6552 = CARTESIAN_POINT ( 'NONE',  ( 4.999999999999998224, -44.99999999999997158, -99.40000000000000568 ) ) ;
#6553 = ORIENTED_EDGE ( 'NONE', *, *, #7973, .F. ) ;
#6554 = CARTESIAN_POINT ( 'NONE',  ( -28.67030704715798350, -37.80000000000000426, 8.395350895058669494 ) ) ;
#6555 = AXIS2_PLACEMENT_3D ( 'NONE', #8674, #2021, #3875 ) ;
#6556 = AXIS2_PLACEMENT_3D ( 'NONE', #6234, #3596, #1104 ) ;
#6557 = VERTEX_POINT ( 'NONE', #6508 ) ;
#6558 = ADVANCED_FACE ( 'NONE', ( #8505, #7093 ), #4363, .F. ) ;
#6559 = CARTESIAN_POINT ( 'NONE',  ( 2.071067811865474173, -39.99999999999997158, -96.85000000000002274 ) ) ;
#6560 = CARTESIAN_POINT ( 'NONE',  ( -31.48612741788231517, -39.30000000000001137, -9.383039235653804155 ) ) ;
#6561 = VECTOR ( 'NONE', #3895, 1000.000000000000000 ) ;
#6562 = CARTESIAN_POINT ( 'NONE',  ( -3.397431688313778952, -41.32060051903346931, -99.99956440458885254 ) ) ;
#6563 = CARTESIAN_POINT ( 'NONE',  ( -33.90612223281073057, -37.10140427513057659, 7.549504333439023718 ) ) ;
#6564 = AXIS2_PLACEMENT_3D ( 'NONE', #5286, #7993, #662 ) ;
#6565 = DIRECTION ( 'NONE',  ( 0.000000000000000000, 1.000000000000000000, -1.224646799147353207E-16 ) ) ;
#6566 = CARTESIAN_POINT ( 'NONE',  ( -26.14108075221394856, -36.60000000000000853, -7.573555455601170827 ) ) ;
#6567 = CARTESIAN_POINT ( 'NONE',  ( 0.000000000000000000, 0.000000000000000000, 0.000000000000000000 ) ) ;
#6568 = LINE ( 'NONE', #1236, #880 ) ;
#6569 = DIRECTION ( 'NONE',  ( 1.000000000000000000, 0.000000000000000000, 0.000000000000000000 ) ) ;
#6570 = ORIENTED_EDGE ( 'NONE', *, *, #4664, .F. ) ;
#6571 = CARTESIAN_POINT ( 'NONE',  ( -37.98859631114233792, -45.84859572486944046, -4.007875659808334490 ) ) ;
#6572 = CARTESIAN_POINT ( 'NONE',  ( -28.51387258211773812, -37.80000000000000426, 9.383039235653802379 ) ) ;
#6573 = CARTESIAN_POINT ( 'NONE',  ( -38.38706344316003793, -34.70140427513057091, -1.382017864820032083 ) ) ;
#6574 = DIRECTION ( 'NONE',  ( 0.000000000000000000, 0.000000000000000000, 1.000000000000000000 ) ) ;
#6575 = LINE ( 'NONE', #2046, #801 ) ;
#6576 = CARTESIAN_POINT ( 'NONE',  ( -37.02382435302582309, -36.24859572486943904, 7.102600956461226467 ) ) ;
#6577 = CARTESIAN_POINT ( 'NONE',  ( -20.13408869516453947, -43.04999999999999005, -1.562606840307983136 ) ) ;
#6578 = DIRECTION ( 'NONE',  ( 0.000000000000000000, 0.000000000000000000, 1.000000000000000000 ) ) ;
#6579 = CARTESIAN_POINT ( 'NONE',  ( -20.00000000000000000, 0.000000000000000000, 80.00000000000002842 ) ) ;
#6580 = CARTESIAN_POINT ( 'NONE',  ( 1.891708078845682595, -40.43301269999998482, -96.29999999890752349 ) ) ;
#6581 =( NAMED_UNIT ( * ) PLANE_ANGLE_UNIT ( ) SI_UNIT ( $, .RADIAN. ) );
#6582 = ORIENTED_EDGE ( 'NONE', *, *, #6158, .T. ) ;
#6583 = LINE ( 'NONE', #4608, #1744 ) ;
#6584 = CARTESIAN_POINT ( 'NONE',  ( -22.45049566656107842, -46.89859572486944472, -3.906122232810846917 ) ) ;
#6585 = CARTESIAN_POINT ( 'NONE',  ( -36.68005392025794009, -29.00140427513058583, -6.754974922286504757 ) ) ;
#6586 = VERTEX_POINT ( 'NONE', #5853 ) ;
#6587 = ORIENTED_EDGE ( 'NONE', *, *, #3395, .F. ) ;
#6588 = CARTESIAN_POINT ( 'NONE',  ( -31.43380250590416125, -44.30140427513057944, -9.391326687552492558 ) ) ;
#6589 = DIRECTION ( 'NONE',  ( -0.000000000000000000, -0.000000000000000000, 1.000000000000000000 ) ) ;
#6590 = DIRECTION ( 'NONE',  ( 0.000000000000000000, -1.000000000000000000, 0.000000000000000000 ) ) ;
#6591 = DIRECTION ( 'NONE',  ( 0.000000000000000000, 0.000000000000000000, 1.000000000000000000 ) ) ;
#6592 = CARTESIAN_POINT ( 'NONE',  ( -4.999999999999998224, -44.99999999999997158, -96.60000000000000853 ) ) ;
#6593 = DIRECTION ( 'NONE',  ( -0.000000000000000000, -0.000000000000000000, -1.000000000000000000 ) ) ;
#6594 = ORIENTED_EDGE ( 'NONE', *, *, #5517, .F. ) ;
#6595 = CARTESIAN_POINT ( 'NONE',  ( -21.17260567462091458, -43.04999999999999005, -1.398121909749242331 ) ) ;
#6596 = EDGE_LOOP ( 'NONE', ( #7704, #5847, #6429 ) ) ;
#6597 = DIRECTION ( 'NONE',  ( -0.000000000000000000, 1.000000000000000000, -0.000000000000000000 ) ) ;
#6598 = ADVANCED_FACE ( 'NONE', ( #419 ), #5724, .T. ) ;
#6599 = CARTESIAN_POINT ( 'NONE',  ( 4.999999999999998224, -42.92893218813448897, -96.84999999781504698 ) ) ;
#6600 = CARTESIAN_POINT ( 'NONE',  ( -38.90016716647221529, -41.84999999999999432, -4.534861676072185155 ) ) ;
#6601 = CARTESIAN_POINT ( 'NONE',  ( 1.891708078845685481, -49.56698729999997255, -99.79999999890752349 ) ) ;
#6602 = CARTESIAN_POINT ( 'NONE',  ( -5.005283159123838921, -45.16039493131476235, -100.0002415582530517 ) ) ;
#6603 = CARTESIAN_POINT ( 'NONE',  ( -38.83610826798580717, -37.55140427513057944, 1.343104241417631073 ) ) ;
#6604 = AXIS2_PLACEMENT_3D ( 'NONE', #2002, #3942, #8139 ) ;
#6605 = CARTESIAN_POINT ( 'NONE',  ( -4.999999999999998224, -42.92893218813448897, -95.84300000002187403 ) ) ;
#6606 = CIRCLE ( 'NONE', #8461, 2.000000000000000888 ) ;
#6607 = CARTESIAN_POINT ( 'NONE',  ( -28.67030704715798350, -37.80000000000000426, 8.395350895058669494 ) ) ;
#6608 = EDGE_CURVE ( 'NONE', #5916, #2059, #8349, .T. ) ;
#6609 = DIRECTION ( 'NONE',  ( -0.000000000000000000, -0.000000000000000000, -1.000000000000000000 ) ) ;
#6610 = LINE ( 'NONE', #7367, #7636 ) ;
#6611 = DIRECTION ( 'NONE',  ( 0.000000000000000000, -1.000000000000000000, 0.000000000000000000 ) ) ;
#6612 = ORIENTED_EDGE ( 'NONE', *, *, #5502, .F. ) ;
#6613 = CARTESIAN_POINT ( 'NONE',  ( 4.200000000000001954, 2.449293598294707893E-16, -2.000000000000000888 ) ) ;
#6614 = CARTESIAN_POINT ( 'NONE',  ( -39.38303923565386100, -38.70000000000000284, -1.486127417882099788 ) ) ;
#6615 = CARTESIAN_POINT ( 'NONE',  ( -28.72263195913613387, -36.80140427513057944, 8.403638346957361449 ) ) ;
#6616 = LINE ( 'NONE', #8656, #2200 ) ;
#6617 = CIRCLE ( 'NONE', #8033, 1.324999999999999956 ) ;
#6618 = CARTESIAN_POINT ( 'NONE',  ( -37.02382435302582309, -33.24859572486943193, 7.102600956461226467 ) ) ;
#6619 = LINE ( 'NONE', #2670, #8590 ) ;
#6620 = DIRECTION ( 'NONE',  ( -0.000000000000000000, 1.000000000000000000, -0.000000000000000000 ) ) ;
#6621 = CARTESIAN_POINT ( 'NONE',  ( -1.891708078845683039, -40.43301269999998482, -98.79999999890753770 ) ) ;
#6622 = SURFACE_SIDE_STYLE ('',( #3334 ) ) ;
#6623 = ORIENTED_EDGE ( 'NONE', *, *, #3777, .F. ) ;
#6624 = DIRECTION ( 'NONE',  ( -0.000000000000000000, -0.000000000000000000, 1.000000000000000000 ) ) ;
#6625 = CARTESIAN_POINT ( 'NONE',  ( -22.01140368885771892, -50.34859572486944046, 4.007875659808335378 ) ) ;
#6626 = CARTESIAN_POINT ( 'NONE',  ( -39.87462524744216807, -31.55140427513057588, 1.507589171976367215 ) ) ;
#6627 = PRESENTATION_LAYER_ASSIGNMENT (  '', '', ( #1718 ) ) ;
#6628 = ORIENTED_EDGE ( 'NONE', *, *, #7092, .T. ) ;
#6629 = EDGE_LOOP ( 'NONE', ( #523, #4744 ) ) ;
#6630 = CARTESIAN_POINT ( 'NONE',  ( -36.68005392025794009, -50.00140427513058938, -6.754974922286504757 ) ) ;
#6631 = SURFACE_STYLE_USAGE ( .BOTH. , #3954 ) ;
#6632 = DIRECTION ( 'NONE',  ( -0.000000000000000000, 1.000000000000000000, -0.000000000000000000 ) ) ;
#6633 = CARTESIAN_POINT ( 'NONE',  ( 4.999999999999998224, -44.99999999999997158, -99.29999999781504982 ) ) ;
#6634 = ORIENTED_EDGE ( 'NONE', *, *, #7673, .T. ) ;
#6635 = DIRECTION ( 'NONE',  ( -1.000000000000000000, 0.000000000000000000, 0.000000000000000000 ) ) ;
#6636 = CARTESIAN_POINT ( 'NONE',  ( 2.071067811865474173, -39.99999999999997158, -99.25000000000000000 ) ) ;
#6637 = ORIENTED_EDGE ( 'NONE', *, *, #2771, .F. ) ;
#6638 = CARTESIAN_POINT ( 'NONE',  ( -36.01040764008574513, -45.00000000000000711, -6.010407640085605685 ) ) ;
#6639 = CIRCLE ( 'NONE', #575, 1.324999999999999956 ) ;
#6640 = AXIS2_PLACEMENT_3D ( 'NONE', #8515, #644, #391 ) ;
#6641 = DIRECTION ( 'NONE',  ( 1.000000000000000000, 0.000000000000000000, 0.000000000000000000 ) ) ;
#6642 = CARTESIAN_POINT ( 'NONE',  ( -4.566987299999998307, -43.10829192115428299, -98.69999999890752918 ) ) ;
#6643 = CARTESIAN_POINT ( 'NONE',  ( -4.999999999999998224, -42.92893218813448897, -99.85000000000002274 ) ) ;
#6644 = CARTESIAN_POINT ( 'NONE',  ( -21.53543802021056663, -39.90000000000000568, -4.312909747525783821 ) ) ;
#6645 = CARTESIAN_POINT ( 'NONE',  ( 4.566987299999998307, -43.10829192115428299, -97.19999999890752918 ) ) ;
#6646 = VECTOR ( 'NONE', #5812, 1000.000000000000000 ) ;
#6647 = CARTESIAN_POINT ( 'NONE',  ( -4.991843310627483099, -44.59989201564595618, -99.99932436085771315 ) ) ;
#6648 =( GEOMETRIC_REPRESENTATION_CONTEXT ( 3 ) GLOBAL_UNCERTAINTY_ASSIGNED_CONTEXT ( ( #5793 ) ) GLOBAL_UNIT_ASSIGNED_CONTEXT ( ( #590, #1300, #3434 ) ) REPRESENTATION_CONTEXT ( 'NONE', 'WORKASPACE' ) );
#6649 = CARTESIAN_POINT ( 'NONE',  ( -26.09387776718931917, -35.60140427513057659, -7.549504333439021941 ) ) ;
#6650 = EDGE_CURVE ( 'NONE', #1784, #2059, #2512, .T. ) ;
#6651 = AXIS2_PLACEMENT_3D ( 'NONE', #3336, #2717, #4830 ) ;
#6652 = CARTESIAN_POINT ( 'NONE',  ( 9.184850993605145972E-16, -49.99999999999997158, -97.19300000002183992 ) ) ;
#6653 = CARTESIAN_POINT ( 'NONE',  ( -37.57355545560112375, -38.40000000000000568, 3.858919247786223305 ) ) ;
#6654 = DIRECTION ( 'NONE',  ( 0.000000000000000000, 0.4999999999999989453, -0.8660254037844392627 ) ) ;
#6655 = CARTESIAN_POINT ( 'NONE',  ( -25.68709025247441602, -48.60000000000000142, -8.464561979789547053 ) ) ;
#6656 =( LENGTH_UNIT ( ) NAMED_UNIT ( * ) SI_UNIT ( .MILLI., .METRE. ) );
#6657 = ORIENTED_EDGE ( 'NONE', *, *, #995, .T. ) ;
#6658 = FACE_OUTER_BOUND ( 'NONE', #5447, .T. ) ;
#6659 = APPLICATION_CONTEXT ( 'automotive_design' ) ;
#6660 = CARTESIAN_POINT ( 'NONE',  ( -36.71751442127229836, -45.00000000000000711, -6.717514421272142044 ) ) ;
#6661 = CARTESIAN_POINT ( 'NONE',  ( -28.54686042191934092, -44.45140427513058512, -8.818680382772479120 ) ) ;
#6662 = AXIS2_PLACEMENT_3D ( 'NONE', #4436, #8490, #3815 ) ;
#6663 = DIRECTION ( 'NONE',  ( 1.000000000000000000, 0.000000000000000000, 0.000000000000000000 ) ) ;
#6664 = CARTESIAN_POINT ( 'NONE',  ( 4.999999999999998224, -44.99999999999997158, -97.00000000000000000 ) ) ;
#6665 = CARTESIAN_POINT ( 'NONE',  ( -39.85719736222883824, -36.54859572486943620, 1.617624508639602388 ) ) ;
#6666 = EDGE_CURVE ( 'NONE', #1476, #7760, #1734, .T. ) ;
#6667 = CARTESIAN_POINT ( 'NONE',  ( -2.071067811865475061, -39.99999999999997158, -99.04999999781504982 ) ) ;
#6668 = DIRECTION ( 'NONE',  ( 0.000000000000000000, 0.000000000000000000, -1.000000000000000000 ) ) ;
#6669 = CARTESIAN_POINT ( 'NONE',  ( 3.229347689422839895, -41.77065231057713390, -95.54999999890752349 ) ) ;
#6670 = SURFACE_STYLE_USAGE ( .BOTH. , #6622 ) ;
#6671 = ORIENTED_EDGE ( 'NONE', *, *, #8524, .F. ) ;
#6672 = LINE ( 'NONE', #626, #5996 ) ;
#6673 = CARTESIAN_POINT ( 'NONE',  ( -33.85891924778610473, -50.10000000000000853, 7.573555455601171715 ) ) ;
#6674 = CARTESIAN_POINT ( 'NONE',  ( -38.44051085762733777, -39.39859572486943762, 4.360112732550414982 ) ) ;
#6675 = CARTESIAN_POINT ( 'NONE',  ( -31.43380250590416125, -44.30140427513057944, -9.391326687552492558 ) ) ;
#6676 = EDGE_LOOP ( 'NONE', ( #6803, #6472, #6291, #770 ) ) ;
#6677 = VERTEX_POINT ( 'NONE', #2389 ) ;
#6678 = CARTESIAN_POINT ( 'NONE',  ( -34.36011273255026310, -46.10140427513058370, 8.440510857627391061 ) ) ;
#6679 = DIRECTION ( 'NONE',  ( -0.000000000000000000, 1.000000000000000000, -0.000000000000000000 ) ) ;
#6680 = CARTESIAN_POINT ( 'NONE',  ( -45.00000000000003553, -44.99999999999997158, 2.099999999999997868 ) ) ;
#6681 = CARTESIAN_POINT ( 'NONE',  ( -3.229347689422840784, -41.77065231057713390, -95.54999999890752349 ) ) ;
#6682 = DIRECTION ( 'NONE',  ( -0.000000000000000000, -0.000000000000000000, -1.000000000000000000 ) ) ;
#6683 = CARTESIAN_POINT ( 'NONE',  ( -2.071067811865475505, -49.99999999999996447, -98.04999999999999716 ) ) ;
#6684 = ORIENTED_EDGE ( 'NONE', *, *, #1265, .F. ) ;
#6685 = CARTESIAN_POINT ( 'NONE',  ( -25.94249218456686279, -43.64999999999999147, 7.963307464738195840 ) ) ;
#6686 = CARTESIAN_POINT ( 'NONE',  ( 2.000000000000000000, 0.000000000000000000, 0.000000000000000000 ) ) ;
#6687 = CIRCLE ( 'NONE', #1911, 9.999999999999998224 ) ;
#6688 = ORIENTED_EDGE ( 'NONE', *, *, #7805, .T. ) ;
#6689 = CARTESIAN_POINT ( 'NONE',  ( 4.566987299999998307, -43.10829192115428299, -98.19999999890752918 ) ) ;
#6690 = CARTESIAN_POINT ( 'NONE',  ( -2.071067811865475061, -39.99999999999997158, -97.44999999781505551 ) ) ;
#6691 = CARTESIAN_POINT ( 'NONE',  ( -21.53543802021056663, -48.90000000000000568, -4.312909747525783821 ) ) ;
#6692 = CARTESIAN_POINT ( 'NONE',  ( -1.891708078845683483, -49.56698729999997255, -98.29999999890752349 ) ) ;
#6693 = PRESENTATION_STYLE_ASSIGNMENT (( #2032 ) ) ;
#6694 = CARTESIAN_POINT ( 'NONE',  ( -36.35910488754074521, -34.25140427513057517, 6.280328284105565650 ) ) ;
#6695 = CARTESIAN_POINT ( 'NONE',  ( -2.071067811865475061, -39.99999999999997158, -96.74300000002187971 ) ) ;
#6696 =( BOUNDED_CURVE ( )  B_SPLINE_CURVE ( 2, ( #5430, #13, #4248, #5521, #2713, #8269, #8140, #3510, #5383 ),
 .UNSPECIFIED., .F., .T. ) 
 B_SPLINE_CURVE_WITH_KNOTS ( ( 3, 2, 2, 2, 3 ),
 ( 0.6428571428571429047, 0.6607142857142856984, 0.6785714285714286031, 0.6964285714285713969, 0.7142857142857143016 ),
 .UNSPECIFIED. ) 
 CURVE ( )  GEOMETRIC_REPRESENTATION_ITEM ( )  RATIONAL_B_SPLINE_CURVE ( ( 1.000000000000000000, 0.9238795325112867385, 1.000000000000000000, 0.9238795325112867385, 1.000000000000000000, 0.9238795325112867385, 1.000000000000000000, 0.9238795325112867385, 1.000000000000000000 ) ) 
 REPRESENTATION_ITEM ( '' )  );
#6697 = CARTESIAN_POINT ( 'NONE',  ( -21.60464910494133406, -31.20000000000000639, 1.329692952841886155 ) ) ;
#6698 = DIRECTION ( 'NONE',  ( 1.000000000000000000, 0.000000000000000000, 0.000000000000000000 ) ) ;
#6699 = EDGE_CURVE ( 'NONE', #4354, #4453, #7782, .T. ) ;
#6700 = FACE_OUTER_BOUND ( 'NONE', #595, .T. ) ;
#6701 = ORIENTED_EDGE ( 'NONE', *, *, #1189, .T. ) ;
#6702 = CARTESIAN_POINT ( 'NONE',  ( 9.184850993605145972E-16, -49.99999999999997158, -99.59999999999999432 ) ) ;
#6703 = CARTESIAN_POINT ( 'NONE',  ( -39.86591130483550671, -47.54999999999999716, 1.562606840307984468 ) ) ;
#6704 = CARTESIAN_POINT ( 'NONE',  ( -28.72263195913613387, -45.80140427513057944, 8.403638346957361449 ) ) ;
#6705 = CIRCLE ( 'NONE', #4752, 11.99999999999979217 ) ;
#6706 = CARTESIAN_POINT ( 'NONE',  ( 29.99999999999997158, 1.102182119232617753E-14, 80.00000000000002842 ) ) ;
#6707 = AXIS2_PLACEMENT_3D ( 'NONE', #5049, #6534, #2413 ) ;
#6708 = DIRECTION ( 'NONE',  ( 0.000000000000000000, 0.000000000000000000, -1.000000000000000000 ) ) ;
#6709 = CARTESIAN_POINT ( 'NONE',  ( -34.26570676250101855, -45.09859572486944046, 8.488613101951703044 ) ) ;
#6710 = FACE_OUTER_BOUND ( 'NONE', #5511, .T. ) ;
#6711 = FACE_OUTER_BOUND ( 'NONE', #139, .T. ) ;
#6712 = CARTESIAN_POINT ( 'NONE',  ( -2.796473189345805913E-16, -40.43301269999997061, -99.64999999890751781 ) ) ;
#6713 = PRESENTATION_LAYER_ASSIGNMENT (  '', '', ( #7848 ) ) ;
#6714 =( NAMED_UNIT ( * ) SI_UNIT ( $, .STERADIAN. ) SOLID_ANGLE_UNIT ( ) );
#6715 = EDGE_LOOP ( 'NONE', ( #2819, #1886 ) ) ;
#6716 = CARTESIAN_POINT ( 'NONE',  ( 30.00000000000000000, 60.00000000000002842, 12.49999999999997335 ) ) ;
#6717 = CARTESIAN_POINT ( 'NONE',  ( -21.60464910494133406, -49.20000000000000995, 1.329692952841886155 ) ) ;
#6718 = CARTESIAN_POINT ( 'NONE',  ( -39.39132668755255651, -36.69859572486944188, -1.433802505903950308 ) ) ;
#6719 = CARTESIAN_POINT ( 'NONE',  ( -31.43380250590416125, -38.30140427513057944, -9.391326687552492558 ) ) ;
#6720 = ORIENTED_EDGE ( 'NONE', *, *, #2327, .F. ) ;
#6721 = VECTOR ( 'NONE', #6867, 1000.000000000000000 ) ;
#6722 = ORIENTED_EDGE ( 'NONE', *, *, #6881, .F. ) ;
#6723 = CARTESIAN_POINT ( 'NONE',  ( -39.37475178375516549, -46.70140427513057801, -1.538452329860249712 ) ) ;
#6724 = FACE_OUTER_BOUND ( 'NONE', #4666, .T. ) ;
#6725 = FACE_OUTER_BOUND ( 'NONE', #8675, .T. ) ;
#6726 = CARTESIAN_POINT ( 'NONE',  ( -4.999999999999998224, -42.92893218813448897, -100.5499999978150498 ) ) ;
#6727 = CARTESIAN_POINT ( 'NONE',  ( 34.83728160242328187, -46.30802241892373416, 11.52630626327733410 ) ) ;
#6728 = FACE_OUTER_BOUND ( 'NONE', #1486, .T. ) ;
#6729 = EDGE_CURVE ( 'NONE', #7212, #4697, #2304, .T. ) ;
#6730 = ORIENTED_EDGE ( 'NONE', *, *, #2970, .T. ) ;
#6731 = CARTESIAN_POINT ( 'NONE',  ( -34.05750781543318340, -48.15000000000001279, -7.963307464738195840 ) ) ;
#6732 = CARTESIAN_POINT ( 'NONE',  ( -31.48612741788231517, -36.30000000000000426, -9.383039235653804155 ) ) ;
#6733 = EDGE_LOOP ( 'NONE', ( #377, #3524, #5043, #7206 ) ) ;
#6734 = CARTESIAN_POINT ( 'NONE',  ( -4.566987299999998307, -44.99999999999997158, -96.24999999890751212 ) ) ;
#6735 = CARTESIAN_POINT ( 'NONE',  ( -2.071067811865475505, -49.99999999999996447, -96.34999999781506119 ) ) ;
#6736 = CARTESIAN_POINT ( 'NONE',  ( -38.46456197978948666, -44.40000000000000568, 4.312909747525784709 ) ) ;
#6737 = CARTESIAN_POINT ( 'NONE',  ( -2.796473189345805913E-16, -40.43301269999997061, -99.44999999890752918 ) ) ;
#6738 = FACE_BOUND ( 'NONE', #8621, .T. ) ;
#6739 = CARTESIAN_POINT ( 'NONE',  ( -22.06198138166579170, -39.35140427513057659, 4.107139971057695682 ) ) ;
#6740 = CARTESIAN_POINT ( 'NONE',  ( 3.535533905932737309, -48.53553390593270933, -95.49300000002185129 ) ) ;
#6741 = CARTESIAN_POINT ( 'NONE',  ( -37.96330746473829976, -41.85000000000000142, -4.057507815433013754 ) ) ;
#6742 = DIRECTION ( 'NONE',  ( -0.000000000000000000, 0.000000000000000000, 1.000000000000000000 ) ) ;
#6743 = CARTESIAN_POINT ( 'NONE',  ( -41.99999999999985789, 0.000000000000000000, -29.65000000000000213 ) ) ;
#6744 = EDGE_LOOP ( 'NONE', ( #7842, #1215 ) ) ;
#6745 = CARTESIAN_POINT ( 'NONE',  ( 34.00000000000000000, 0.000000000000000000, 0.000000000000000000 ) ) ;
#6746 = CARTESIAN_POINT ( 'NONE',  ( -21.53543802021056663, -48.90000000000000568, -4.312909747525783821 ) ) ;
#6747 = CARTESIAN_POINT ( 'NONE',  ( -28.72263195913613387, -48.80140427513057233, 8.403638346957361449 ) ) ;
#6748 = CIRCLE ( 'NONE', #3668, 1.649999999999998579 ) ;
#6749 = DIRECTION ( 'NONE',  ( -1.000000000000000000, 0.000000000000000000, 0.000000000000000000 ) ) ;
#6750 = DIRECTION ( 'NONE',  ( 1.000000000000000000, 0.000000000000000000, 0.000000000000000000 ) ) ;
#6751 = CARTESIAN_POINT ( 'NONE',  ( -37.02382435302582309, -51.24859572486943193, 7.102600956461226467 ) ) ;
#6752 = PLANE ( 'NONE',  #6604 ) ;
#6753 = CARTESIAN_POINT ( 'NONE',  ( -31.48612741788231517, -33.30000000000000426, -9.383039235653804155 ) ) ;
#6754 = ORIENTED_EDGE ( 'NONE', *, *, #7148, .T. ) ;
#6755 = CARTESIAN_POINT ( 'NONE',  ( 3.535533905932737309, -48.53553390593270933, -98.70000000000000284 ) ) ;
#6756 = CARTESIAN_POINT ( 'NONE',  ( -21.17260567462091458, -49.04999999999999716, -1.398121909749242331 ) ) ;
#6757 = CARTESIAN_POINT ( 'NONE',  ( -23.24502507771338600, -35.49859572486943193, 6.680053920257780220 ) ) ;
#6758 = CARTESIAN_POINT ( 'NONE',  ( -21.12512167993187973, -45.35140427513057659, 4.584493831696868860 ) ) ;
#6759 = ADVANCED_FACE ( 'NONE', ( #7754 ), #8215, .F. ) ;
#6760 = CIRCLE ( 'NONE', #857, 12.49999999999996980 ) ;
#6761 = ORIENTED_EDGE ( 'NONE', *, *, #8716, .F. ) ;
#6762 = ORIENTED_EDGE ( 'NONE', *, *, #5229, .T. ) ;
#6763 = CARTESIAN_POINT ( 'NONE',  ( -38.48861310195163554, -43.40140427513058796, 4.265706762501153548 ) ) ;
#6764 = CYLINDRICAL_SURFACE ( 'NONE', #4330, 2.000000000000000888 ) ;
#6765 = CARTESIAN_POINT ( 'NONE',  ( -3.061616997868382155E-16, -39.99999999999997158, -99.89999999781504414 ) ) ;
#6766 = CARTESIAN_POINT ( 'NONE',  ( -25.64110105645932336, 10.00000000000000178, -25.00000000000000000 ) ) ;
#6767 = CARTESIAN_POINT ( 'NONE',  ( -3.535533905932735532, -48.53553390593270933, -96.39999999781505835 ) ) ;
#6768 = ORIENTED_EDGE ( 'NONE', *, *, #8065, .T. ) ;
#6769 = EDGE_CURVE ( 'NONE', #3127, #4571, #5665, .T. ) ;
#6770 = CARTESIAN_POINT ( 'NONE',  ( -37.96330746473829976, -47.85000000000000853, -4.057507815433013754 ) ) ;
#6771 = CARTESIAN_POINT ( 'NONE',  ( -31.56260684030781505, -37.94999999999998153, 9.865911304835510265 ) ) ;
#6772 = VERTEX_POINT ( 'NONE', #4577 ) ;
#6773 = EDGE_CURVE ( 'NONE', #2955, #5525, #6551, .T. ) ;
#6774 = ORIENTED_EDGE ( 'NONE', *, *, #3928, .F. ) ;
#6775 = CARTESIAN_POINT ( 'NONE',  ( 4.566987299999998307, -44.99999999999997158, -97.44999999890751496 ) ) ;
#6776 = CARTESIAN_POINT ( 'NONE',  ( 1.932551333443697450, -39.99999999999997158, -100.0466559163918419 ) ) ;
#6777 = CARTESIAN_POINT ( 'NONE',  ( -39.86591130483550671, -47.54999999999999716, 1.562606840307984468 ) ) ;
#6778 = CARTESIAN_POINT ( 'NONE',  ( 1.891708078845682595, -40.43301269999998482, -97.09999999890753486 ) ) ;
#6779 = AXIS2_PLACEMENT_3D ( 'NONE', #684, #2597, #4616 ) ;
#6780 = DIRECTION ( 'NONE',  ( -1.000000000000000000, -0.000000000000000000, -0.000000000000000000 ) ) ;
#6781 = CARTESIAN_POINT ( 'NONE',  ( -21.61293655684001536, -45.20140427513059223, 1.382017864820032971 ) ) ;
#6782 = CIRCLE ( 'NONE', #8213, 11.99999999999979217 ) ;
#6783 = CARTESIAN_POINT ( 'NONE',  ( 5.000000000000000000, -47.07106781186545419, -96.24300000002185129 ) ) ;
#6784 = AXIS2_PLACEMENT_3D ( 'NONE', #8545, #3702, #6427 ) ;
#6785 = CARTESIAN_POINT ( 'NONE',  ( -23.98959235991431171, -46.50000000000000711, 6.010407640085604797 ) ) ;
#6786 = CARTESIAN_POINT ( 'NONE',  ( 25.50988976140734366, -47.22366675470350117, 11.66649199791332592 ) ) ;
#6787 = DIRECTION ( 'NONE',  ( 0.000000000000000000, 0.000000000000000000, 1.000000000000000000 ) ) ;
#6788 = EDGE_CURVE ( 'NONE', #2418, #5152, #4906, .T. ) ;
#6789 = SHAPE_DEFINITION_REPRESENTATION ( #1703, #2265 ) ;
#6790 = ORIENTED_EDGE ( 'NONE', *, *, #495, .F. ) ;
#6791 = DIRECTION ( 'NONE',  ( 0.000000000000000000, 0.000000000000000000, 1.000000000000000000 ) ) ;
#6792 = CARTESIAN_POINT ( 'NONE',  ( -25.46513832392765408, -43.64999999999999147, 8.900167166472096270 ) ) ;
#6793 = CARTESIAN_POINT ( 'NONE',  ( -36.35910488754074521, -49.25140427513058938, 6.280328284105565650 ) ) ;
#6794 = EDGE_CURVE ( 'NONE', #8290, #8403, #5624, .T. ) ;
#6795 = CIRCLE ( 'NONE', #2309, 1.324999999999999734 ) ;
#6796 = PRODUCT_DEFINITION ( 'UNKNOWN', '', #6074, #1772 ) ;
#6797 = CARTESIAN_POINT ( 'NONE',  ( -4.566987299999998307, -44.99999999999997158, -95.44999999890751496 ) ) ;
#6798 = FACE_OUTER_BOUND ( 'NONE', #8315, .T. ) ;
#6799 = CARTESIAN_POINT ( 'NONE',  ( -28.46154767013959486, -44.79859572486943620, 9.374751783755112200 ) ) ;
#6800 = DIRECTION ( 'NONE',  ( 1.000000000000000000, 0.000000000000000000, 0.000000000000000000 ) ) ;
#6801 = CIRCLE ( 'NONE', #5532, 1.649999999999998579 ) ;
#6802 = CARTESIAN_POINT ( 'NONE',  ( -21.09983283352783801, -31.34999999999999432, 4.534861676072186043 ) ) ;
#6803 = ORIENTED_EDGE ( 'NONE', *, *, #4940, .F. ) ;
#6804 = DIRECTION ( 'NONE',  ( -1.000000000000000000, -0.000000000000000000, -0.000000000000000000 ) ) ;
#6805 = ORIENTED_EDGE ( 'NONE', *, *, #2080, .T. ) ;
#6806 = CARTESIAN_POINT ( 'NONE',  ( -31.34310424141748896, -32.94859572486944188, 8.836108267985801845 ) ) ;
#6807 = CARTESIAN_POINT ( 'NONE',  ( -21.55948914237271907, -40.89859572486943762, -4.360112732550413206 ) ) ;
#6808 = CARTESIAN_POINT ( 'NONE',  ( -25.63988726744978663, -38.60140427513057659, -8.440510857627391061 ) ) ;
#6809 = SHAPE_REPRESENTATION ( 'Body', ( #2554 ), #5211 ) ;
#6810 = AXIS2_PLACEMENT_3D ( 'NONE', #822, #4795, #776 ) ;
#6811 = ORIENTED_EDGE ( 'NONE', *, *, #8589, .T. ) ;
#6812 = EDGE_LOOP ( 'NONE', ( #5932, #152, #2981, #5571, #3052 ) ) ;
#6813 = CARTESIAN_POINT ( 'NONE',  ( -34.99999999999997868, -45.00000000000000000, 11.45643923738958847 ) ) ;
#6814 = CARTESIAN_POINT ( 'NONE',  ( -4.999999999999998224, -42.92893218813448897, -98.94999999781504130 ) ) ;
#6815 = DIRECTION ( 'NONE',  ( -0.000000000000000000, -0.000000000000000000, 1.000000000000000000 ) ) ;
#6816 = DIRECTION ( 'NONE',  ( 0.000000000000000000, 0.000000000000000000, 1.000000000000000000 ) ) ;
#6817 = ORIENTED_EDGE ( 'NONE', *, *, #4327, .T. ) ;
#6818 = CARTESIAN_POINT ( 'NONE',  ( -38.40363834695740053, -33.69859572486942767, -1.277368040863739118 ) ) ;
#6819 = CARTESIAN_POINT ( 'NONE',  ( -25.68709025247441602, -30.60000000000000142, -8.464561979789547053 ) ) ;
#6820 = ORIENTED_EDGE ( 'NONE', *, *, #1464, .F. ) ;
#6821 = SURFACE_STYLE_FILL_AREA ( #5585 ) ;
#6822 = CARTESIAN_POINT ( 'NONE',  ( 8.389419568037416259E-16, -49.56698729999997255, -98.44999999890752918 ) ) ;
#6823 = CARTESIAN_POINT ( 'NONE',  ( -3.061616997868382155E-16, -39.99999999999997158, -99.89999999781504414 ) ) ;
#6824 = CARTESIAN_POINT ( 'NONE',  ( -37.06321265474346660, -50.24999999999998579, 7.063212654743582952 ) ) ;
#6825 = CARTESIAN_POINT ( 'NONE',  ( 4.566987300000000083, -46.89170807884565306, -98.09999999890752065 ) ) ;
#6826 =( NAMED_UNIT ( * ) SI_UNIT ( $, .STERADIAN. ) SOLID_ANGLE_UNIT ( ) );
#6827 = CARTESIAN_POINT ( 'NONE',  ( -22.40239342223677355, -41.90140427513058086, -3.811716262761597473 ) ) ;
#6828 = CARTESIAN_POINT ( 'NONE',  ( -3.535533905932736864, -41.46446609406723383, -99.09300000002185982 ) ) ;
#6829 = VECTOR ( 'NONE', #7265, 1000.000000000000114 ) ;
#6830 = CARTESIAN_POINT ( 'NONE',  ( -23.68028341417693738, -45.75000000000000000, -6.319716585823200283 ) ) ;
#6831 = CARTESIAN_POINT ( 'NONE',  ( -42.00000000000006395, 0.000000000000000000, -25.00000000000000000 ) ) ;
#6832 = APPLICATION_PROTOCOL_DEFINITION ( 'draft international standard', 'automotive_design', 1998, #2741 ) ;
#6833 = EDGE_LOOP ( 'NONE', ( #4129, #6105 ) ) ;
#6834 = LINE ( 'NONE', #8392, #5103 ) ;
#6835 = CARTESIAN_POINT ( 'NONE',  ( -34.31290974752564438, -47.10000000000000142, 8.464561979789547053 ) ) ;
#6836 = CARTESIAN_POINT ( 'NONE',  ( -28.67030704715798350, -31.80000000000000782, 8.395350895058669494 ) ) ;
#6837 = CARTESIAN_POINT ( 'NONE',  ( 25.03353697015359458, -44.33501760501477662, 11.47123432380332808 ) ) ;
#6838 = CIRCLE ( 'NONE', #7263, 1.000000000000000888 ) ;
#6839 = CARTESIAN_POINT ( 'NONE',  ( -26.64110105645932336, 8.000000000000000000, 125.0000000000000000 ) ) ;
#6840 = CARTESIAN_POINT ( 'NONE',  ( -21.07454398712378918, -44.34859572486944046, 4.485229520447505003 ) ) ;
#6841 = DIRECTION ( 'NONE',  ( -1.000000000000000000, 0.000000000000000000, 0.000000000000000000 ) ) ;
#6842 = CARTESIAN_POINT ( 'NONE',  ( -37.06321265474346660, -35.25000000000000000, 7.063212654743582952 ) ) ;
#6843 = VECTOR ( 'NONE', #5210, 1000.000000000000000 ) ;
#6844 = FILL_AREA_STYLE ('',( #6232 ) ) ;
#6845 = VERTEX_POINT ( 'NONE', #3392 ) ;
#6846 = CARTESIAN_POINT ( 'NONE',  ( 2.000000000000000000, -1.773042676681341634, 2.493664996716660198E-15 ) ) ;
#6847 = ORIENTED_EDGE ( 'NONE', *, *, #3921, .F. ) ;
#6848 = CARTESIAN_POINT ( 'NONE',  ( -23.95213185889994989, -38.49859572486943904, 5.972947139071243861 ) ) ;
#6849 = CARTESIAN_POINT ( 'NONE',  ( -20.14280263777121149, -44.04859572486944330, -1.617624508639600833 ) ) ;
#6850 = CARTESIAN_POINT ( 'NONE',  ( -34.48522952044771017, -38.15140427513058086, -8.925456012876139766 ) ) ;
#6851 = AXIS2_PLACEMENT_3D ( 'NONE', #1830, #6410, #5091 ) ;
#6852 = ORIENTED_EDGE ( 'NONE', *, *, #7534, .F. ) ;
#6853 = CARTESIAN_POINT ( 'NONE',  ( -3.229347689422840784, -41.77065231057713390, -96.94999999890751496 ) ) ;
#6854 = CARTESIAN_POINT ( 'NONE',  ( -31.48612741788231517, -30.30000000000000782, -9.383039235653804155 ) ) ;
#6855 = CARTESIAN_POINT ( 'NONE',  ( -33.97112193926510315, -41.94466314146776398, 11.85397847079114975 ) ) ;
#6856 = CARTESIAN_POINT ( 'NONE',  ( -4.566987299999997418, -46.89170807884566727, -96.99999999890751212 ) ) ;
#6857 = CARTESIAN_POINT ( 'NONE',  ( -30.00000000000002842, 0.000000000000000000, -29.65000000000000213 ) ) ;
#6858 = DIRECTION ( 'NONE',  ( 0.000000000000000000, 0.000000000000000000, 1.000000000000000000 ) ) ;
#6859 = VERTEX_POINT ( 'NONE', #1347 ) ;
#6860 = AXIS2_PLACEMENT_3D ( 'NONE', #319, #396, #5039 ) ;
#6861 = CARTESIAN_POINT ( 'NONE',  ( -37.54950433343896776, -36.39859572486944472, 3.906122232810848249 ) ) ;
#6862 = CARTESIAN_POINT ( 'NONE',  ( -36.71751442127229836, -33.00000000000000711, -6.717514421272142044 ) ) ;
#6863 = ORIENTED_EDGE ( 'NONE', *, *, #1726, .F. ) ;
#6864 = CARTESIAN_POINT ( 'NONE',  ( -37.06321265474346660, -50.24999999999998579, 7.063212654743582952 ) ) ;
#6865 = CARTESIAN_POINT ( 'NONE',  ( 0.000000000000000000, -44.99999999999997158, -95.00000000000000000 ) ) ;
#6866 = CARTESIAN_POINT ( 'NONE',  ( -2.796473189345805913E-16, -40.43301269999997061, -99.64999999890751781 ) ) ;
#6867 = DIRECTION ( 'NONE',  ( -1.000000000000000000, -0.000000000000000000, -0.000000000000000000 ) ) ;
#6868 = CARTESIAN_POINT ( 'NONE',  ( -41.99999999999996447, -22.00000000000000000, 80.00000000000002842 ) ) ;
#6869 = CARTESIAN_POINT ( 'NONE',  ( 1.891708078845682595, -40.43301269999998482, -97.89999999890753202 ) ) ;
#6870 = EDGE_CURVE ( 'NONE', #7760, #5393, #8107, .T. ) ;
#6871 = CARTESIAN_POINT ( 'NONE',  ( -26.09387776718931917, -41.60140427513058370, -7.549504333439021941 ) ) ;
#6872 = ADVANCED_FACE ( 'NONE', ( #5227 ), #7258, .F. ) ;
#6873 = CARTESIAN_POINT ( 'NONE',  ( 2.071067811865474173, -39.99999999999997158, -96.04999999999999716 ) ) ;
#6874 = CARTESIAN_POINT ( 'NONE',  ( 3.229347689422839895, -41.77065231057713390, -96.34999999890753486 ) ) ;
#6875 = CARTESIAN_POINT ( 'NONE',  ( -37.96330746473829976, -47.85000000000000142, -4.057507815433013754 ) ) ;
#6876 = CARTESIAN_POINT ( 'NONE',  ( 3.535533905932736420, -41.46446609406723383, -95.99999999781503845 ) ) ;
#6877 = ITEM_DEFINED_TRANSFORMATION ( 'NONE', 'NONE', #2564,  #2554 ) ;
#6878 = ORIENTED_EDGE ( 'NONE', *, *, #4845, .F. ) ;
#6879 = CARTESIAN_POINT ( 'NONE',  ( -30.00000000000000000, -45.00000000000000000, 30.00000000000000000 ) ) ;
#6880 = CARTESIAN_POINT ( 'NONE',  ( -33.85891924778610473, -41.10000000000000142, 7.573555455601171715 ) ) ;
#6881 = EDGE_CURVE ( 'NONE', #3552, #1476, #1447, .T. ) ;
#6882 = DIRECTION ( 'NONE',  ( 0.000000000000000000, 0.000000000000000000, 1.000000000000000000 ) ) ;
#6883 = CARTESIAN_POINT ( 'NONE',  ( -50.00000000000002842, -44.99999999999997158, 0.000000000000000000 ) ) ;
#6884 = CARTESIAN_POINT ( 'NONE',  ( -31.53845232986046554, -49.29859572486945041, -9.374751783755117529 ) ) ;
#6885 = DIRECTION ( 'NONE',  ( -1.000000000000000000, 0.000000000000000000, 0.000000000000000000 ) ) ;
#6886 = CARTESIAN_POINT ( 'NONE',  ( -31.56260684030781505, -31.95000000000000639, 9.865911304835508489 ) ) ;
#6887 = ORIENTED_EDGE ( 'NONE', *, *, #5860, .T. ) ;
#6888 = FACE_OUTER_BOUND ( 'NONE', #3368, .T. ) ;
#6889 = ORIENTED_EDGE ( 'NONE', *, *, #5761, .F. ) ;
#6890 = CARTESIAN_POINT ( 'NONE',  ( -21.18131961722757595, -41.04859572486944330, -1.453139578080854699 ) ) ;
#6891 = ADVANCED_FACE ( 'NONE', ( #1219 ), #3916, .T. ) ;
#6892 = CARTESIAN_POINT ( 'NONE',  ( -37.02382435302582309, -45.24859572486943904, 7.102600956461226467 ) ) ;
#6893 = CARTESIAN_POINT ( 'NONE',  ( -34.36011273255026310, -49.10140427513058370, 8.440510857627391061 ) ) ;
#6894 = VECTOR ( 'NONE', #5469, 1000.000000000000000 ) ;
#6895 = ORIENTED_EDGE ( 'NONE', *, *, #1709, .T. ) ;
#6896 = CARTESIAN_POINT ( 'NONE',  ( -3.229347689422840784, -41.77065231057713390, -95.34999999890753486 ) ) ;
#6897 = FILL_AREA_STYLE_COLOUR ( '', #3987 ) ;
#6898 = FACE_OUTER_BOUND ( 'NONE', #8313, .T. ) ;
#6899 = CIRCLE ( 'NONE', #3536, 2.149999999999985256 ) ;
#6900 = CARTESIAN_POINT ( 'NONE',  ( -3.229347689422839451, -48.22934768942280925, -96.94999999890751496 ) ) ;
#6901 = CARTESIAN_POINT ( 'NONE',  ( 4.000000000000000000, 0.000000000000000000, 0.000000000000000000 ) ) ;
#6902 = DIRECTION ( 'NONE',  ( 0.000000000000000000, 0.000000000000000000, 1.000000000000000000 ) ) ;
#6903 = ORIENTED_EDGE ( 'NONE', *, *, #495, .T. ) ;
#6904 = CARTESIAN_POINT ( 'NONE',  ( -38.82739432537914581, -47.54999999999999716, 1.398121909749243441 ) ) ;
#6905 = CARTESIAN_POINT ( 'NONE',  ( -31.48612741788231517, -30.30000000000000782, -9.383039235653804155 ) ) ;
#6906 = VECTOR ( 'NONE', #268, 1000.000000000000000 ) ;
#6907 = EDGE_LOOP ( 'NONE', ( #8228, #2806, #1472, #4875 ) ) ;
#6908 = CARTESIAN_POINT ( 'NONE',  ( -37.06321265474346660, -47.25000000000000711, 7.063212654743582952 ) ) ;
#6909 = CARTESIAN_POINT ( 'NONE',  ( 50.00000000000002842, -30.00000000000000000, 60.00000000000002842 ) ) ;
#6910 = CARTESIAN_POINT ( 'NONE',  ( 1.891708078845682595, -40.43301269999998482, -99.69999999890752918 ) ) ;
#6911 = DIRECTION ( 'NONE',  ( 1.000000000000000000, 0.000000000000000000, 0.000000000000000000 ) ) ;
#6912 = CARTESIAN_POINT ( 'NONE',  ( -36.71751442127229836, -51.00000000000000711, -6.717514421272142044 ) ) ;
#6913 = CARTESIAN_POINT ( 'NONE',  ( 4.566987300000000083, -46.89170807884565306, -99.69999999890752918 ) ) ;
#6914 = ORIENTED_EDGE ( 'NONE', *, *, #6382, .F. ) ;
#6915 = CARTESIAN_POINT ( 'NONE',  ( -37.59760657776328685, -46.40140427513058086, 3.811716262761598362 ) ) ;
#6916 = CARTESIAN_POINT ( 'NONE',  ( -3.535533905932736864, -41.46446609406723383, -95.90000000000000568 ) ) ;
#6917 = CARTESIAN_POINT ( 'NONE',  ( -26.64110105645932336, -9.999999999999998224, -25.00000000000000000 ) ) ;
#6918 = CARTESIAN_POINT ( 'NONE',  ( -23.98959235991431171, -49.50000000000000711, 6.010407640085604797 ) ) ;
#6919 = PRODUCT_DEFINITION_FORMATION_WITH_SPECIFIED_SOURCE ( 'ANY', '', #1628, .NOT_KNOWN. ) ;
#6920 = DIRECTION ( 'NONE',  ( 1.000000000000000000, -0.000000000000000000, 0.000000000000000000 ) ) ;
#6921 = EDGE_CURVE ( 'NONE', #1925, #1663, #3347, .T. ) ;
#6922 = SHAPE_DEFINITION_REPRESENTATION ( #2973, #6471 ) ;
#6923 = DIRECTION ( 'NONE',  ( -0.000000000000000000, -0.000000000000000000, -1.000000000000000000 ) ) ;
#6924 = CARTESIAN_POINT ( 'NONE',  ( -28.67030704715798350, -34.80000000000000426, 8.395350895058669494 ) ) ;
#6925 = AXIS2_PLACEMENT_3D ( 'NONE', #3134, #303, #3176 ) ;
#6926 = CARTESIAN_POINT ( 'NONE',  ( -26.94291110594769734, -41.03022111473443090, 12.12354317000653836 ) ) ;
#6927 = DIRECTION ( 'NONE',  ( 0.5150380749100560429, 0.000000000000000000, -0.8571673007021112234 ) ) ;
#6928 = CARTESIAN_POINT ( 'NONE',  ( -21.09983283352784156, -34.35000000000000853, 4.534861676072186043 ) ) ;
#6929 = CARTESIAN_POINT ( 'NONE',  ( 4.999999999999998224, -44.99999999999997158, -97.79999999999999716 ) ) ;
#6930 = CARTESIAN_POINT ( 'NONE',  ( -22.93678734525658314, -30.75000000000000000, -7.063212654743582064 ) ) ;
#6931 = VECTOR ( 'NONE', #1906, 1000.000000000000227 ) ;
#6932 =( LENGTH_UNIT ( ) NAMED_UNIT ( * ) SI_UNIT ( .MILLI., .METRE. ) );
#6933 = VERTEX_POINT ( 'NONE', #8713 ) ;
#6934 = LINE ( 'NONE', #1602, #1076 ) ;
#6935 = ORIENTED_EDGE ( 'NONE', *, *, #3126, .F. ) ;
#6936 = AXIS2_PLACEMENT_3D ( 'NONE', #67, #1929, #8670 ) ;
#6937 = CARTESIAN_POINT ( 'NONE',  ( -31.38201786482021305, -40.29859572486944330, -8.387063443159975762 ) ) ;
#6938 = CARTESIAN_POINT ( 'NONE',  ( -25.46513832392765408, -31.65000000000000568, 8.900167166472096270 ) ) ;
#6939 = CARTESIAN_POINT ( 'NONE',  ( -33.90612223281073057, -34.10140427513057659, 7.549504333439023718 ) ) ;
#6940 = EDGE_CURVE ( 'NONE', #5592, #2848, #7608, .T. ) ;
#6941 = CARTESIAN_POINT ( 'NONE',  ( -3.229347689422839451, -48.22934768942280925, -96.74999999890752633 ) ) ;
#6942 = VECTOR ( 'NONE', #7426, 1000.000000000000114 ) ;
#6943 = CYLINDRICAL_SURFACE ( 'NONE', #2927, 4.999999999999998224 ) ;
#6944 = CARTESIAN_POINT ( 'NONE',  ( 1.891708078845682595, -40.43301269999998482, -98.09999999890750644 ) ) ;
#6945 = DIRECTION ( 'NONE',  ( 0.000000000000000000, -1.000000000000000000, 0.000000000000000000 ) ) ;
#6946 = DIRECTION ( 'NONE',  ( -1.000000000000000000, 0.000000000000000000, 0.000000000000000000 ) ) ;
#6947 = EDGE_LOOP ( 'NONE', ( #1934, #2278, #3234, #6671 ) ) ;
#6948 = CARTESIAN_POINT ( 'NONE',  ( -28.65689575858256077, -37.44859572486943478, -8.836108267985801845 ) ) ;
#6949 = AXIS2_PLACEMENT_3D ( 'NONE', #4562, #3377, #6051 ) ;
#6950 = CARTESIAN_POINT ( 'NONE',  ( -21.53543802021056663, -42.90000000000000568, -4.312909747525783821 ) ) ;
#6951 = APPLICATION_CONTEXT ( 'automotive_design' ) ;
#6952 = VERTEX_POINT ( 'NONE', #2947 ) ;
#6953 = CARTESIAN_POINT ( 'NONE',  ( -36.68005392025794009, -29.00140427513058583, -6.754974922286504757 ) ) ;
#6954 = CARTESIAN_POINT ( 'NONE',  ( -1.891708078845683705, -49.56698729999997255, -100.0999999989075206 ) ) ;
#6955 = AXIS2_PLACEMENT_3D ( 'NONE', #6901, #2113, #2287 ) ;
#6956 = CARTESIAN_POINT ( 'NONE',  ( -3.061616997868382155E-16, -39.99999999999997158, -99.09999999781504698 ) ) ;
#6957 = DIRECTION ( 'NONE',  ( -1.000000000000000000, 0.000000000000000000, 0.000000000000000000 ) ) ;
#6958 = CARTESIAN_POINT ( 'NONE',  ( 4.566987299999998307, -43.10829192115428299, -98.79999999890753770 ) ) ;
#6959 = ORIENTED_EDGE ( 'NONE', *, *, #4668, .T. ) ;
#6960 = CARTESIAN_POINT ( 'NONE',  ( -28.60187809025093841, -30.44999999999999574, -8.827394325379140483 ) ) ;
#6961 = ADVANCED_FACE ( 'NONE', ( #4175 ), #3564, .T. ) ;
#6962 = CARTESIAN_POINT ( 'NONE',  ( -3.535533905932735532, -48.53553390593270933, -99.69300000002185413 ) ) ;
#6963 = CARTESIAN_POINT ( 'NONE',  ( -4.566987299999998307, -44.99999999999997158, -95.24999999890752633 ) ) ;
#6964 = CARTESIAN_POINT ( 'NONE',  ( -26.64110105645932336, -7.999999999999996447, 124.0000000000000000 ) ) ;
#6965 = DIRECTION ( 'NONE',  ( -0.000000000000000000, 0.000000000000000000, 1.000000000000000000 ) ) ;
#6966 = CARTESIAN_POINT ( 'NONE',  ( 29.99999999999997158, -57.51075773784449296, -1.102182119232617753E-14 ) ) ;
#6967 = CARTESIAN_POINT ( 'NONE',  ( -31.39812190974910422, -34.95000000000000995, 8.827394325379140483 ) ) ;
#6968 = VECTOR ( 'NONE', #962, 1000.000000000000000 ) ;
#6969 = CARTESIAN_POINT ( 'NONE',  ( -29.67090686519078346, -40.00809359540125598, 12.49675575313102271 ) ) ;
#6970 = EDGE_CURVE ( 'NONE', #282, #4270, #3707, .T. ) ;
#6971 = CARTESIAN_POINT ( 'NONE',  ( 4.999999999999998224, -42.92893218813449607, -98.54999999999999716 ) ) ;
#6972 = CARTESIAN_POINT ( 'NONE',  ( -38.90016716647221529, -35.84999999999998721, -4.534861676072185155 ) ) ;
#6973 = CARTESIAN_POINT ( 'NONE',  ( 3.072733599874575727, -41.00166578800908468, -100.0000000000000142 ) ) ;
#6974 = CARTESIAN_POINT ( 'NONE',  ( -25.46513832392766119, -40.65000000000000568, 8.900167166472096270 ) ) ;
#6975 = ORIENTED_EDGE ( 'NONE', *, *, #8464, .F. ) ;
#6976 = CARTESIAN_POINT ( 'NONE',  ( -42.00000000000006395, 0.000000000000000000, -26.00000000000000355 ) ) ;
#6977 = ORIENTED_EDGE ( 'NONE', *, *, #4037, .F. ) ;
#6978 = CARTESIAN_POINT ( 'NONE',  ( -38.81868038277247734, -36.54859572486943620, 1.453139578080855365 ) ) ;
#6979 = AXIS2_PLACEMENT_3D ( 'NONE', #2777, #6286, #6902 ) ;
#6980 = CARTESIAN_POINT ( 'NONE',  ( -31.53845232986046554, -49.29859572486945041, -9.374751783755117529 ) ) ;
#6981 = CARTESIAN_POINT ( 'NONE',  ( -24.02705286092866643, -30.50140427513058583, 6.047868141099968398 ) ) ;
#6982 = AXIS2_PLACEMENT_3D ( 'NONE', #8226, #2799, #54 ) ;
#6983 = EDGE_CURVE ( 'NONE', #3221, #1195, #1021, .T. ) ;
#6984 = CARTESIAN_POINT ( 'NONE',  ( -2.796473189345805913E-16, -40.43301269999997061, -96.24999999890752633 ) ) ;
#6985 = DIRECTION ( 'NONE',  ( -0.000000000000000000, -0.000000000000000000, -1.000000000000000000 ) ) ;
#6986 = CARTESIAN_POINT ( 'NONE',  ( -30.65892580703207670, -40.03249052150655274, 12.48689449661284279 ) ) ;
#6987 = CARTESIAN_POINT ( 'NONE',  ( 3.229347689422841228, -48.22934768942280925, -97.54999999890752349 ) ) ;
#6988 = FACE_OUTER_BOUND ( 'NONE', #5463, .T. ) ;
#6989 = CARTESIAN_POINT ( 'NONE',  ( 1.891708078845685481, -49.56698729999997255, -98.39999999890753202 ) ) ;
#6990 = DIRECTION ( 'NONE',  ( 0.000000000000000000, 0.000000000000000000, 1.000000000000000000 ) ) ;
#6991 = ORIENTED_EDGE ( 'NONE', *, *, #6940, .T. ) ;
#6992 = CARTESIAN_POINT ( 'NONE',  ( -22.01140368885771892, -41.34859572486944757, 4.007875659808335378 ) ) ;
#6993 = CARTESIAN_POINT ( 'NONE',  ( -21.09983283352784156, -46.34999999999998721, 4.534861676072186043 ) ) ;
#6994 = ORIENTED_EDGE ( 'NONE', *, *, #4689, .T. ) ;
#6995 = CARTESIAN_POINT ( 'NONE',  ( -25.46513832392765408, -49.64999999999999147, 8.900167166472096270 ) ) ;
#6996 = CARTESIAN_POINT ( 'NONE',  ( 50.00000000000002842, -44.99999999999997158, 2.099999999999997868 ) ) ;
#6997 = DIRECTION ( 'NONE',  ( -0.000000000000000000, -0.000000000000000000, -1.000000000000000000 ) ) ;
#6999 = EDGE_CURVE ( 'NONE', #112, #5042, #2162, .T. ) ;
#6998 = AXIS2_PLACEMENT_3D ( 'NONE', #5123, #394, #1633 ) ;
#7000 = CARTESIAN_POINT ( 'NONE',  ( -2.071067811865475061, -39.99999999999997158, -99.84999999781504698 ) ) ;
#7001 = CARTESIAN_POINT ( 'NONE',  ( -20.61696076434619584, -49.20000000000000995, 1.486127417882100676 ) ) ;
#7002 = PRESENTATION_LAYER_ASSIGNMENT (  '', '', ( #4896 ) ) ;
#7003 = CARTESIAN_POINT ( 'NONE',  ( -3.229347689422840784, -41.77065231057713390, -98.54999999890752349 ) ) ;
#7004 = ORIENTED_EDGE ( 'NONE', *, *, #1924, .F. ) ;
#7005 = CARTESIAN_POINT ( 'NONE',  ( -22.42644454439892598, -33.90000000000000568, -3.858919247786222861 ) ) ;
#7006 = AXIS2_PLACEMENT_3D ( 'NONE', #5105, #1763, #5020 ) ;
#7007 = CARTESIAN_POINT ( 'NONE',  ( -3.535533905932735532, -48.53553390593270933, -98.89300000002185698 ) ) ;
#7008 = CARTESIAN_POINT ( 'NONE',  ( -30.00000000000002842, -9.999999999999998224, -24.00000000000000000 ) ) ;
#7009 = CARTESIAN_POINT ( 'NONE',  ( 4.999999999999998224, -42.92893218813448897, -97.64999999781504414 ) ) ;
#7010 = DIRECTION ( 'NONE',  ( -1.000000000000000000, 0.000000000000000000, 0.000000000000000000 ) ) ;
#7011 = CARTESIAN_POINT ( 'NONE',  ( -3.061616997868382155E-16, -39.99999999999997158, -100.6999999978150555 ) ) ;
#7012 = CARTESIAN_POINT ( 'NONE',  ( -38.82739432537914581, -35.55000000000001137, 1.398121909749243441 ) ) ;
#7013 = CARTESIAN_POINT ( 'NONE',  ( 0.000000000000000000, 0.8865213383406683745, -1.535500000000000753 ) ) ;
#7014 = DIRECTION ( 'NONE',  ( 0.000000000000000000, 1.000000000000000000, 0.000000000000000000 ) ) ;
#7015 = CARTESIAN_POINT ( 'NONE',  ( -31.56260684030781505, -34.95000000000000995, 9.865911304835510265 ) ) ;
#7016 = CLOSED_SHELL ( 'NONE', ( #154, #3867, #3263, #5209 ) ) ;
#7017 = LINE ( 'NONE', #3759, #1654 ) ;
#7018 = CARTESIAN_POINT ( 'NONE',  ( -20.61696076434619584, -37.20000000000000284, 1.486127417882100676 ) ) ;
#7019 = EDGE_CURVE ( 'NONE', #4340, #1975, #587, .T. ) ;
#7020 = EDGE_LOOP ( 'NONE', ( #1350, #680 ) ) ;
#7021 = FACE_OUTER_BOUND ( 'NONE', #8244, .T. ) ;
#7022 = ORIENTED_EDGE ( 'NONE', *, *, #3749, .T. ) ;
#7023 = CARTESIAN_POINT ( 'NONE',  ( -25.89286002894218086, -41.64859572486943762, 7.938018618334153231 ) ) ;
#7024 = CARTESIAN_POINT ( 'NONE',  ( -39.39132668755255651, -51.69859572486944188, -1.433802505903950308 ) ) ;
#7025 = CARTESIAN_POINT ( 'NONE',  ( -39.87462524744216807, -46.55140427513058654, 1.507589171976367215 ) ) ;
#7026 = EDGE_CURVE ( 'NONE', #1975, #4340, #5545, .T. ) ;
#7027 = CARTESIAN_POINT ( 'NONE',  ( -4.566987299999998307, -43.10829192115428299, -100.0999999989075349 ) ) ;
#7028 = UNCERTAINTY_MEASURE_WITH_UNIT (LENGTH_MEASURE( 1.000000000000000082E-05 ), #6053, 'distance_accuracy_value', 'NONE');
#7029 = DIRECTION ( 'NONE',  ( -0.000000000000000000, -0.000000000000000000, 1.000000000000000000 ) ) ;
#7030 = CARTESIAN_POINT ( 'NONE',  ( 8.389419568037416259E-16, -49.56698729999997255, -98.44999999890752918 ) ) ;
#7031 = DIRECTION ( 'NONE',  ( -0.000000000000000000, 1.000000000000000000, 0.000000000000000000 ) ) ;
#7032 = CARTESIAN_POINT ( 'NONE',  ( -4.566987299999998307, -44.99999999999997158, -97.84999999890752065 ) ) ;
#7033 = VECTOR ( 'NONE', #2585, 1000.000000000000000 ) ;
#7034 = EDGE_LOOP ( 'NONE', ( #6540, #6502 ) ) ;
#7035 = EDGE_CURVE ( 'NONE', #2752, #3221, #1567, .T. ) ;
#7036 = CARTESIAN_POINT ( 'NONE',  ( -34.10713997105786888, -43.14859572486943762, -7.938018618334151455 ) ) ;
#7037 = CARTESIAN_POINT ( 'NONE',  ( -37.06321265474346660, -41.25000000000000711, 7.063212654743582952 ) ) ;
#7038 = VERTEX_POINT ( 'NONE', #1441 ) ;
#7039 = CARTESIAN_POINT ( 'NONE',  ( -37.06321265474346660, -44.25000000000000000, 7.063212654743582952 ) ) ;
#7040 = AXIS2_PLACEMENT_3D ( 'NONE', #4392, #1876, #7160 ) ;
#7042 = CARTESIAN_POINT ( 'NONE',  ( 4.999999999999998224, -44.99999999999997158, -96.89999999781505835 ) ) ;
#7041 =( BOUNDED_CURVE ( )  B_SPLINE_CURVE ( 2, ( #4300, #8238, #5573, #1521, #8321 ),
 .UNSPECIFIED., .F., .T. ) 
 B_SPLINE_CURVE_WITH_KNOTS ( ( 3, 2, 3 ),
 ( 0.8571428571428572063, 0.8750000000000000000, 0.8928571428571429047 ),
 .UNSPECIFIED. ) 
 CURVE ( )  GEOMETRIC_REPRESENTATION_ITEM ( )  RATIONAL_B_SPLINE_CURVE ( ( 0.9999999999999995559, 0.9238795325112871826, 1.000000000000000000, 0.9238795325112867385, 1.000000000000000000 ) ) 
 REPRESENTATION_ITEM ( '' )  );
#7043 = CARTESIAN_POINT ( 'NONE',  ( 4.999999999999998224, -44.99999999999997158, -98.49999999781503845 ) ) ;
#7044 = DIRECTION ( 'NONE',  ( 6.123233995736960786E-17, -1.000000000000000000, 0.000000000000000000 ) ) ;
#7045 = EDGE_CURVE ( 'NONE', #2202, #8551, #909, .T. ) ;
#7046 = CARTESIAN_POINT ( 'NONE',  ( -39.84999999999998010, -22.00000000000000000, 60.00000000000002842 ) ) ;
#7047 = CARTESIAN_POINT ( 'NONE',  ( 3.535533905932736420, -41.46446609406723383, -96.10000000000000853 ) ) ;
#7048 = ORIENTED_EDGE ( 'NONE', *, *, #7899, .F. ) ;
#7049 = PRODUCT ( 'BR-006', 'BR-006', '', ( #5418 ) ) ;
#7050 = CARTESIAN_POINT ( 'NONE',  ( -23.98959235991431171, -34.50000000000000000, 6.010407640085604797 ) ) ;
#7051 = ADVANCED_FACE ( 'NONE', ( #69 ), #4263, .F. ) ;
#7052 = CIRCLE ( 'NONE', #1712, 2.149999999999985256 ) ;
#7053 = ORIENTED_EDGE ( 'NONE', *, *, #257, .F. ) ;
#7054 = CARTESIAN_POINT ( 'NONE',  ( -3.229347689422840784, -41.77065231057713390, -95.34999999890753486 ) ) ;
#7055 = CARTESIAN_POINT ( 'NONE',  ( -4.999999999999998224, -42.92893218813448897, -95.74999999781503845 ) ) ;
#7056 = B_SPLINE_CURVE_WITH_KNOTS ( 'NONE', 3,
 ( #2270, #1420, #6837, #845, #2227, #228, #3589, #1507, #4950, #53, #4201, #3545, #1465, #4286, #7588, #2842, #6226, #187, #805, #2798 ),
 .UNSPECIFIED., .F., .F.,
 ( 4, 2, 2, 2, 2, 2, 2, 2, 2, 4 ),
 ( 0.007902764345171071902, 0.008889850383257314262, 0.009876936421343554887, 0.01086402245942979725, 0.01185110849751603787, 0.01283819453560228023, 0.01333173755464540575, 0.01382528057368853300, 0.01481236661177478577, 0.01579945264986103853 ),
 .UNSPECIFIED. ) ;
#7057 = DIRECTION ( 'NONE',  ( 0.000000000000000000, 0.000000000000000000, -1.000000000000000000 ) ) ;
#7058 = FACE_OUTER_BOUND ( 'NONE', #7745, .T. ) ;
#7059 = CARTESIAN_POINT ( 'NONE',  ( -36.01040764008574513, -36.00000000000000711, -6.010407640085605685 ) ) ;
#7060 = DIRECTION ( 'NONE',  ( 1.000000000000000000, 0.000000000000000000, 0.000000000000000000 ) ) ;
#7061 = CARTESIAN_POINT ( 'NONE',  ( 1.891708078845682595, -40.43301269999998482, -95.69999999890751496 ) ) ;
#7062 = PRODUCT_DEFINITION_FORMATION_WITH_SPECIFIED_SOURCE ( 'ANY', '', #3671, .NOT_KNOWN. ) ;
#7063 = CARTESIAN_POINT ( 'NONE',  ( -22.42644454439892598, -30.90000000000000924, -3.858919247786222861 ) ) ;
#7064 = CARTESIAN_POINT ( 'NONE',  ( -28.51387258211773812, -37.80000000000000426, 9.383039235653802379 ) ) ;
#7065 = CYLINDRICAL_SURFACE ( 'NONE', #5305, 4.999999999999973355 ) ;
#7066 = CARTESIAN_POINT ( 'NONE',  ( -21.09983283352783801, -43.35000000000000853, 4.534861676072186043 ) ) ;
#7067 = SURFACE_SIDE_STYLE ('',( #278 ) ) ;
#7068 = VECTOR ( 'NONE', #3088, 1000.000000000000000 ) ;
#7069 = ORIENTED_EDGE ( 'NONE', *, *, #8065, .F. ) ;
#7070 = EDGE_CURVE ( 'NONE', #8290, #207, #7562, .T. ) ;
#7071 = ORIENTED_EDGE ( 'NONE', *, *, #6281, .T. ) ;
#7072 = CARTESIAN_POINT ( 'NONE',  ( -36.04786814110010340, -48.99859572486944614, -5.972947139071243861 ) ) ;
#7073 = CARTESIAN_POINT ( 'NONE',  ( -39.85719736222883824, -51.54859572486944330, 1.617624508639602388 ) ) ;
#7074 = AXIS2_PLACEMENT_3D ( 'NONE', #4458, #7352, #5690 ) ;
#7075 = CARTESIAN_POINT ( 'NONE',  ( -38.87487832006816291, -46.85140427513056949, -4.584493831696867971 ) ) ;
#7076 = LINE ( 'NONE', #1035, #8411 ) ;
#7077 = CARTESIAN_POINT ( 'NONE',  ( 30.16445806793351636, -39.99999999999998579, 12.49999999999996625 ) ) ;
#7078 = CARTESIAN_POINT ( 'NONE',  ( -34.53486167607238144, -33.15000000000001279, -8.900167166472096270 ) ) ;
#7079 = AXIS2_PLACEMENT_3D ( 'NONE', #4448, #3089, #6339 ) ;
#7080 = DIRECTION ( 'NONE',  ( -0.000000000000000000, -0.000000000000000000, 1.000000000000000000 ) ) ;
#7081 = DIRECTION ( 'NONE',  ( 0.000000000000000000, 0.000000000000000000, 1.000000000000000000 ) ) ;
#7082 = AXIS2_PLACEMENT_3D ( 'NONE', #8194, #4215, #2283 ) ;
#7083 = CARTESIAN_POINT ( 'NONE',  ( 4.566987300000000083, -46.89170807884565306, -95.89999999890753202 ) ) ;
#7084 = CARTESIAN_POINT ( 'NONE',  ( 42.00000000000000711, 48.00000000000002842, 23.64999999999992042 ) ) ;
#7085 = ORIENTED_EDGE ( 'NONE', *, *, #5468, .F. ) ;
#7086 = CARTESIAN_POINT ( 'NONE',  ( -28.61798213517984024, -44.79859572486943620, 8.387063443159973986 ) ) ;
#7087 = CARTESIAN_POINT ( 'NONE',  ( -34.53486167607238144, -48.15000000000001279, -8.900167166472096270 ) ) ;
#7088 = ORIENTED_EDGE ( 'NONE', *, *, #5457, .F. ) ;
#7089 = CARTESIAN_POINT ( 'NONE',  ( -34.36011273255026310, -34.10140427513057659, 8.440510857627391061 ) ) ;
#7090 = DIRECTION ( 'NONE',  ( 1.000000000000000000, 0.000000000000000000, 0.000000000000000000 ) ) ;
#7091 = DIRECTION ( 'NONE',  ( -1.000000000000000000, 0.000000000000000000, 0.000000000000000000 ) ) ;
#7092 = EDGE_CURVE ( 'NONE', #2769, #6055, #8197, .T. ) ;
#7093 = FACE_OUTER_BOUND ( 'NONE', #6075, .T. ) ;
#7094 = CARTESIAN_POINT ( 'NONE',  ( -3.535533905932736864, -41.46446609406723383, -95.10000000000000853 ) ) ;
#7095 = EDGE_LOOP ( 'NONE', ( #4009, #2159 ) ) ;
#7096 = CARTESIAN_POINT ( 'NONE',  ( -21.60464910494133406, -37.20000000000000284, 1.329692952841886155 ) ) ;
#7097 = SHAPE_REPRESENTATION ( 'socket head cap screw_iso_ISO 4762 M4 x 30 - 20N', ( #2554 ), #7620 ) ;
#7098 = CIRCLE ( 'NONE', #3308, 2.149999999999985256 ) ;
#7099 = ORIENTED_EDGE ( 'NONE', *, *, #6388, .T. ) ;
#7100 = CARTESIAN_POINT ( 'NONE',  ( -2.071067811865475061, -39.99999999999997158, -97.54999999999998295 ) ) ;
#7101 = CARTESIAN_POINT ( 'NONE',  ( -2.071067811865475505, -49.99999999999996447, -97.94999999781504130 ) ) ;
#7102 = DIRECTION ( 'NONE',  ( -0.000000000000000000, -0.000000000000000000, -1.000000000000000000 ) ) ;
#7103 = CONTEXT_DEPENDENT_SHAPE_REPRESENTATION ( #2125, #1594 ) ;
#7104 = CARTESIAN_POINT ( 'NONE',  ( 50.00000000000002842, -59.99999999999997158, -30.00000000000000000 ) ) ;
#7105 = CARTESIAN_POINT ( 'NONE',  ( -4.999999999999998224, -44.99999999999997158, -99.69999999781505551 ) ) ;
#7106 = DIRECTION ( 'NONE',  ( 1.000000000000000000, 0.000000000000000000, 0.000000000000000000 ) ) ;
#7107 = CARTESIAN_POINT ( 'NONE',  ( -31.56260684030781505, -31.95000000000000639, 9.865911304835510265 ) ) ;
#7108 = DIRECTION ( 'NONE',  ( 0.000000000000000000, 0.000000000000000000, 1.000000000000000000 ) ) ;
#7109 = CARTESIAN_POINT ( 'NONE',  ( -21.53543802021056663, -42.90000000000000568, -4.312909747525783821 ) ) ;
#7110 = ORIENTED_EDGE ( 'NONE', *, *, #4569, .T. ) ;
#7111 = CARTESIAN_POINT ( 'NONE',  ( -23.95213185889994989, -47.49859572486944614, 5.972947139071243861 ) ) ;
#7112 = CARTESIAN_POINT ( 'NONE',  ( -22.93678734525658314, -39.74999999999999289, -7.063212654743582952 ) ) ;
#7113 = CARTESIAN_POINT ( 'NONE',  ( -23.64089511245930098, -41.75140427513057517, -6.280328284105564762 ) ) ;
#7114 = CIRCLE ( 'NONE', #782, 4.999999999999998224 ) ;
#7115 = CARTESIAN_POINT ( 'NONE',  ( 4.566987299999998307, -44.99999999999997158, -99.64999999890753202 ) ) ;
#7116 = CARTESIAN_POINT ( 'NONE',  ( 11.32499999999999929, 1.386912500034377407E-15, 0.000000000000000000 ) ) ;
#7117 = CARTESIAN_POINT ( 'NONE',  ( -39.38303923565386100, -35.70000000000000995, -1.486127417882099788 ) ) ;
#7118 = PLANE ( 'NONE',  #1123 ) ;
#7119 = CARTESIAN_POINT ( 'NONE',  ( -33.35889894354067309, -8.999999999999998224, 125.0000000000000000 ) ) ;
#7120 = CARTESIAN_POINT ( 'NONE',  ( 8.389419568037416259E-16, -49.56698729999997255, -96.04999999890752349 ) ) ;
#7121 =( LENGTH_UNIT ( ) NAMED_UNIT ( * ) SI_UNIT ( .MILLI., .METRE. ) );
#7122 = ORIENTED_EDGE ( 'NONE', *, *, #8340, .F. ) ;
#7123 = SURFACE_STYLE_USAGE ( .BOTH. , #492 ) ;
#7124 = CARTESIAN_POINT ( 'NONE',  ( -36.04786814110010340, -45.99859572486943904, -5.972947139071243861 ) ) ;
#7125 = CARTESIAN_POINT ( 'NONE',  ( -25.51477047955235378, -33.65140427513057375, 8.925456012876139766 ) ) ;
#7126 = ORIENTED_EDGE ( 'NONE', *, *, #5588, .T. ) ;
#7127 = CARTESIAN_POINT ( 'NONE',  ( -39.87462524744216807, -34.55140427513057233, 1.507589171976367215 ) ) ;
#7128 = CYLINDRICAL_SURFACE ( 'NONE', #6011, 7.499999999999999112 ) ;
#7129 = LINE ( 'NONE', #1092, #3840 ) ;
#7130 = CARTESIAN_POINT ( 'NONE',  ( 4.999999999999996447, -47.07106781186543998, -95.45000000000000284 ) ) ;
#7131 = AXIS2_PLACEMENT_3D ( 'NONE', #1557, #898, #6275 ) ;
#7132 = DIRECTION ( 'NONE',  ( 1.000000000000000000, 0.000000000000000000, 0.000000000000000000 ) ) ;
#7133 = CARTESIAN_POINT ( 'NONE',  ( 3.535533905932736420, -41.46446609406723383, -96.90000000000000568 ) ) ;
#7134 = ORIENTED_EDGE ( 'NONE', *, *, #1692, .T. ) ;
#7135 = CARTESIAN_POINT ( 'NONE',  ( -34.05750781543318340, -30.15000000000000213, -7.963307464738195840 ) ) ;
#7136 = AXIS2_PLACEMENT_3D ( 'NONE', #3240, #6750, #6708 ) ;
#7137 = ORIENTED_EDGE ( 'NONE', *, *, #5864, .F. ) ;
#7138 = EDGE_CURVE ( 'NONE', #4408, #8429, #1044, .T. ) ;
#7139 = CARTESIAN_POINT ( 'NONE',  ( 3.535533905932736420, -41.46446609406723383, -98.50000000000000000 ) ) ;
#7140 = VECTOR ( 'NONE', #6120, 1000.000000000000000 ) ;
#7141 = FACE_OUTER_BOUND ( 'NONE', #33, .T. ) ;
#7142 = CARTESIAN_POINT ( 'NONE',  ( 0.8856097000871558933, -49.92917650584813316, -100.0008279209158388 ) ) ;
#7143 = CYLINDRICAL_SURFACE ( 'NONE', #6640, 1.000000000000000888 ) ;
#7144 = EDGE_CURVE ( 'NONE', #1056, #5746, #4004, .T. ) ;
#7145 = CARTESIAN_POINT ( 'NONE',  ( -35.35889894354067309, -7.999999999999996447, -25.00000000000000000 ) ) ;
#7146 = CARTESIAN_POINT ( 'NONE',  ( -4.999999999999998224, -44.99999999999997158, -98.19999999999998863 ) ) ;
#7147 = CARTESIAN_POINT ( 'NONE',  ( 2.000000000000000000, 0.8865213383406683745, -1.535500000000000753 ) ) ;
#7148 = EDGE_CURVE ( 'NONE', #1046, #2177, #3160, .T. ) ;
#7149 = CARTESIAN_POINT ( 'NONE',  ( -36.71751442127229836, -45.00000000000000711, -6.717514421272142044 ) ) ;
#7150 =( LENGTH_UNIT ( ) NAMED_UNIT ( * ) SI_UNIT ( .MILLI., .METRE. ) );
#7151 = ORIENTED_EDGE ( 'NONE', *, *, #2496, .T. ) ;
#7152 = CARTESIAN_POINT ( 'NONE',  ( -21.07454398712378918, -32.34859572486942625, 4.485229520447505003 ) ) ;
#7153 = CARTESIAN_POINT ( 'NONE',  ( -38.46456197978948666, -41.40000000000000568, 4.312909747525784709 ) ) ;
#7154 = CARTESIAN_POINT ( 'NONE',  ( -33.90612223281073057, -43.10140427513058370, 7.549504333439023718 ) ) ;
#7155 = EDGE_CURVE ( 'NONE', #5681, #772, #7521, .T. ) ;
#7156 = CARTESIAN_POINT ( 'NONE',  ( 3.229347689422841228, -48.22934768942280925, -99.74999999890752633 ) ) ;
#7157 = LINE ( 'NONE', #3034, #2645 ) ;
#7158 = CARTESIAN_POINT ( 'NONE',  ( -39.39132668755255651, -33.69859572486942767, -1.433802505903950308 ) ) ;
#7159 = CARTESIAN_POINT ( 'NONE',  ( -28.43739315969223824, -33.45000000000000995, -9.865911304835512041 ) ) ;
#7160 = DIRECTION ( 'NONE',  ( 0.000000000000000000, 0.000000000000000000, 1.000000000000000000 ) ) ;
#7161 = FACE_OUTER_BOUND ( 'NONE', #8606, .T. ) ;
#7162 = CARTESIAN_POINT ( 'NONE',  ( 4.566987299999998307, -43.10829192115428299, -95.79999999890752349 ) ) ;
#7163 = EDGE_CURVE ( 'NONE', #3431, #7971, #2034, .T. ) ;
#7164 = VERTEX_POINT ( 'NONE', #8241 ) ;
#7165 = CARTESIAN_POINT ( 'NONE',  ( -4.999999999999998224, -44.99999999999997158, -95.00000000000000000 ) ) ;
#7166 = CARTESIAN_POINT ( 'NONE',  ( -22.97617564697422665, -34.74859572486943904, -7.102600956461224690 ) ) ;
#7167 = CARTESIAN_POINT ( 'NONE',  ( -25.51477047955235378, -30.65140427513057730, 8.925456012876139766 ) ) ;
#7168 = EDGE_LOOP ( 'NONE', ( #346, #5403 ) ) ;
#7169 = CARTESIAN_POINT ( 'NONE',  ( -39.37475178375516549, -31.70140427513057091, -1.538452329860249712 ) ) ;
#7170 = CARTESIAN_POINT ( 'NONE',  ( -41.99999999999996447, -22.00000000000000000, 60.00000000000002842 ) ) ;
#7171 = LINE ( 'NONE', #7215, #6236 ) ;
#7172 = LINE ( 'NONE', #6550, #3696 ) ;
#7173 = FACE_OUTER_BOUND ( 'NONE', #6446, .T. ) ;
#7174 = CARTESIAN_POINT ( 'NONE',  ( -4.999999999999997335, -47.07106781186546129, -97.35000000000000853 ) ) ;
#7175 = EDGE_CURVE ( 'NONE', #1617, #6859, #2477, .T. ) ;
#7176 = ORIENTED_EDGE ( 'NONE', *, *, #4128, .T. ) ;
#7177 = CARTESIAN_POINT ( 'NONE',  ( -25.94249218456686279, -40.65000000000000568, 7.963307464738195840 ) ) ;
#7178 = ADVANCED_FACE ( 'NONE', ( #6988 ), #3647, .F. ) ;
#7179 = PRODUCT_RELATED_PRODUCT_CATEGORY ( 'part', '', ( #7676 ) ) ;
#7180 = AXIS2_PLACEMENT_3D ( 'NONE', #1067, #1643, #356 ) ;
#7181 = ORIENTED_EDGE ( 'NONE', *, *, #1157, .F. ) ;
#7182 = CARTESIAN_POINT ( 'NONE',  ( -3.535533905932736864, -41.46446609406723383, -98.29999999999999716 ) ) ;
#7183 = CARTESIAN_POINT ( 'NONE',  ( 4.712883770844864983, -46.76680472316598980, -99.99969226647576193 ) ) ;
#7184 = DIRECTION ( 'NONE',  ( -1.000000000000000000, 0.000000000000000000, 0.000000000000000000 ) ) ;
#7185 = CARTESIAN_POINT ( 'NONE',  ( -41.99999999999996447, 22.00000000000000000, 80.00000000000002842 ) ) ;
#7186 = AXIS2_PLACEMENT_3D ( 'NONE', #3669, #5073, #3096 ) ;
#7187 = CARTESIAN_POINT ( 'NONE',  ( 50.00000000000002842, 30.00000000000000000, 80.00000000000002842 ) ) ;
#7188 = CARTESIAN_POINT ( 'NONE',  ( -25.94249218456686279, -31.65000000000000568, 7.963307464738194952 ) ) ;
#7189 = CARTESIAN_POINT ( 'NONE',  ( 42.00000000000000711, 48.00000000000002842, -21.99999999999992184 ) ) ;
#7190 =( GEOMETRIC_REPRESENTATION_CONTEXT ( 3 ) GLOBAL_UNCERTAINTY_ASSIGNED_CONTEXT ( ( #608 ) ) GLOBAL_UNIT_ASSIGNED_CONTEXT ( ( #1837, #3246, #2628 ) ) REPRESENTATION_CONTEXT ( 'NONE', 'WORKASPACE' ) );
#7191 = DIRECTION ( 'NONE',  ( 0.000000000000000000, -0.4999999999999992784, 0.8660254037844389297 ) ) ;
#7192 = DIRECTION ( 'NONE',  ( 0.000000000000000000, 1.000000000000000000, 0.000000000000000000 ) ) ;
#7193 = ORIENTED_EDGE ( 'NONE', *, *, #6394, .F. ) ;
#7194 = CARTESIAN_POINT ( 'NONE',  ( -21.59636165304264921, -44.19859572486944899, 1.277368040863740228 ) ) ;
#7195 = CARTESIAN_POINT ( 'NONE',  ( -34.53486167607238144, -36.15000000000001279, -8.900167166472096270 ) ) ;
#7196 = CARTESIAN_POINT ( 'NONE',  ( -22.40239342223677355, -35.90140427513058086, -3.811716262761597473 ) ) ;
#7197 =( GEOMETRIC_REPRESENTATION_CONTEXT ( 3 ) GLOBAL_UNCERTAINTY_ASSIGNED_CONTEXT ( ( #5551 ) ) GLOBAL_UNIT_ASSIGNED_CONTEXT ( ( #7150, #321, #3635 ) ) REPRESENTATION_CONTEXT ( 'NONE', 'WORKASPACE' ) );
#7198 = CARTESIAN_POINT ( 'NONE',  ( 3.535533905932736420, -41.46446609406723383, -96.10000000000000853 ) ) ;
#7199 = CARTESIAN_POINT ( 'NONE',  ( -41.99999999999996447, 60.00000000000002842, -22.00000000000000000 ) ) ;
#7200 = CARTESIAN_POINT ( 'NONE',  ( -22.97617564697422665, -40.74859572486943904, -7.102600956461224690 ) ) ;
#7201 = CARTESIAN_POINT ( 'NONE',  ( -25.46513832392765408, -37.65000000000000568, 8.900167166472096270 ) ) ;
#7202 = CARTESIAN_POINT ( 'NONE',  ( -34.99999999999997868, -45.00000000000000000, -30.00100000000000122 ) ) ;
#7203 = DIRECTION ( 'NONE',  ( 1.000000000000000000, -0.000000000000000000, -0.000000000000000000 ) ) ;
#7204 = CARTESIAN_POINT ( 'NONE',  ( 8.389419568037416259E-16, -49.56698729999997255, -99.24999999890751212 ) ) ;
#7205 = CIRCLE ( 'NONE', #3417, 0.2000000000000000944 ) ;
#7206 = ORIENTED_EDGE ( 'NONE', *, *, #4736, .T. ) ;
#7207 = CARTESIAN_POINT ( 'NONE',  ( -41.99999999999996447, 60.00000000000002842, -22.00000000000000000 ) ) ;
#7208 = CARTESIAN_POINT ( 'NONE',  ( -23.95213185889994989, -47.49859572486944614, 5.972947139071243861 ) ) ;
#7209 = CARTESIAN_POINT ( 'NONE',  ( -21.51138689804841420, -32.90140427513058086, -4.265706762501151772 ) ) ;
#7210 = EDGE_CURVE ( 'NONE', #4999, #4084, #5962, .T. ) ;
#7211 = EDGE_LOOP ( 'NONE', ( #4212, #7718, #5730, #733 ) ) ;
#7212 = VERTEX_POINT ( 'NONE', #6370 ) ;
#7213 = CARTESIAN_POINT ( 'NONE',  ( -20.12537475255788522, -36.05140427513057944, -1.507589171976365439 ) ) ;
#7214 = CARTESIAN_POINT ( 'NONE',  ( -34.96759668750374317, -45.65721116879225860, 11.47074269425085724 ) ) ;
#7215 = CARTESIAN_POINT ( 'NONE',  ( -31.74999999999995737, 0.000000000000000000, 3.500000000000000000 ) ) ;
#7216 = FACE_OUTER_BOUND ( 'NONE', #3722, .T. ) ;
#7217 = DIRECTION ( 'NONE',  ( -0.000000000000000000, 1.000000000000000000, -0.000000000000000000 ) ) ;
#7218 = CARTESIAN_POINT ( 'NONE',  ( 4.999999999999998224, -42.92893218813448897, -96.15000000000000568 ) ) ;
#7219 = EDGE_LOOP ( 'NONE', ( #4977, #8220, #642, #3527 ) ) ;
#7220 = CARTESIAN_POINT ( 'NONE',  ( -22.03669253526174998, -46.34999999999998721, 4.057507815433014642 ) ) ;
#7221 = CIRCLE ( 'NONE', #8360, 12.49999999999998757 ) ;
#7222 = EDGE_LOOP ( 'NONE', ( #2673, #491, #373 ) ) ;
#7223 = CARTESIAN_POINT ( 'NONE',  ( -4.999999999999997335, -47.07106781186546129, -98.95000000000000284 ) ) ;
#7224 =( GEOMETRIC_REPRESENTATION_CONTEXT ( 3 ) GLOBAL_UNCERTAINTY_ASSIGNED_CONTEXT ( ( #2832 ) ) GLOBAL_UNIT_ASSIGNED_CONTEXT ( ( #3818, #5891, #410 ) ) REPRESENTATION_CONTEXT ( 'NONE', 'WORKASPACE' ) );
#7225 = CARTESIAN_POINT ( 'NONE',  ( 1.999693926619486195, -49.61910733158132558, -99.99999752325564373 ) ) ;
#7226 = EDGE_CURVE ( 'NONE', #5746, #7878, #2455, .T. ) ;
#7227 = CARTESIAN_POINT ( 'NONE',  ( -21.61293655684001536, -33.20140427513057091, 1.382017864820032971 ) ) ;
#7228 = VECTOR ( 'NONE', #3078, 1000.000000000000000 ) ;
#7229 = APPLICATION_CONTEXT ( 'automotive_design' ) ;
#7230 = CARTESIAN_POINT ( 'NONE',  ( -4.999999999999998224, -44.99999999999997158, -97.29999999781504982 ) ) ;
#7231 = CARTESIAN_POINT ( 'NONE',  ( -21.17260567462091103, -34.04999999999999005, -1.398121909749241887 ) ) ;
#7232 = LINE ( 'NONE', #1235, #5444 ) ;
#7233 = DIRECTION ( 'NONE',  ( 1.000000000000000000, 0.000000000000000000, 0.000000000000000000 ) ) ;
#7234 = CARTESIAN_POINT ( 'NONE',  ( 50.00000000000002842, 0.000000000000000000, 0.000000000000000000 ) ) ;
#7235 = ORIENTED_EDGE ( 'NONE', *, *, #3131, .F. ) ;
#7236 = CARTESIAN_POINT ( 'NONE',  ( -37.54950433343896776, -45.39859572486944472, 3.906122232810848249 ) ) ;
#7237 = CARTESIAN_POINT ( 'NONE',  ( -28.43739315969223824, -33.45000000000000995, -9.865911304835512041 ) ) ;
#7238 = CARTESIAN_POINT ( 'NONE',  ( -36.35910488754074521, -43.25140427513058228, 6.280328284105565650 ) ) ;
#7239 = ADVANCED_FACE ( 'NONE', ( #1793 ), #7784, .T. ) ;
#7240 = LINE ( 'NONE', #4599, #6561 ) ;
#7241 = DIRECTION ( 'NONE',  ( -0.000000000000000000, 1.000000000000000000, -0.000000000000000000 ) ) ;
#7242 = CARTESIAN_POINT ( 'NONE',  ( -28.46154767013959486, -41.79859572486943620, 9.374751783755112200 ) ) ;
#7243 = CARTESIAN_POINT ( 'NONE',  ( -20.61696076434619584, -37.20000000000000284, 1.486127417882100676 ) ) ;
#7244 = DIRECTION ( 'NONE',  ( -0.000000000000000000, 1.000000000000000000, -0.000000000000000000 ) ) ;
#7245 = LINE ( 'NONE', #5216, #1598 ) ;
#7246 = CARTESIAN_POINT ( 'NONE',  ( -1.891708078845683483, -49.56698729999997255, -95.89999999890753202 ) ) ;
#7247 = ORIENTED_EDGE ( 'NONE', *, *, #7805, .F. ) ;
#7248 = CARTESIAN_POINT ( 'NONE',  ( -17.99999999999998579, 1.469576158976828483E-15, -26.00000000000000355 ) ) ;
#7249 = CARTESIAN_POINT ( 'NONE',  ( -22.01140368885771892, -47.34859572486942625, 4.007875659808335378 ) ) ;
#7250 = CARTESIAN_POINT ( 'NONE',  ( -31.56260684030781505, -49.95000000000000995, 9.865911304835510265 ) ) ;
#7251 = EDGE_CURVE ( 'NONE', #1887, #5183, #7098, .T. ) ;
#7252 = EDGE_CURVE ( 'NONE', #6055, #6288, #2416, .T. ) ;
#7253 = EDGE_LOOP ( 'NONE', ( #253, #1667, #5861, #2650, #3248 ) ) ;
#7254 = CARTESIAN_POINT ( 'NONE',  ( -25.51477047955235378, -45.65140427513058086, 8.925456012876139766 ) ) ;
#7255 = AXIS2_PLACEMENT_3D ( 'NONE', #1242, #8088, #6574 ) ;
#7256 = LINE ( 'NONE', #2425, #7641 ) ;
#7257 = FACE_OUTER_BOUND ( 'NONE', #322, .T. ) ;
#7258 = CYLINDRICAL_SURFACE ( 'NONE', #4121, 2.149999999999985256 ) ;
#7259 = CARTESIAN_POINT ( 'NONE',  ( -3.061616997868382155E-16, -39.99999999999997158, -98.40000000000000568 ) ) ;
#7260 = ORIENTED_EDGE ( 'NONE', *, *, #2646, .T. ) ;
#7261 = CARTESIAN_POINT ( 'NONE',  ( -28.67030704715798350, -40.80000000000000426, 8.395350895058669494 ) ) ;
#7262 = ADVANCED_FACE ( 'NONE', ( #290 ), #3732, .F. ) ;
#7263 = AXIS2_PLACEMENT_3D ( 'NONE', #2322, #7184, #8358 ) ;
#7264 = ORIENTED_EDGE ( 'NONE', *, *, #428, .T. ) ;
#7265 = DIRECTION ( 'NONE',  ( -0.7071067811865355823, 0.000000000000000000, 0.7071067811865595631 ) ) ;
#7266 = CARTESIAN_POINT ( 'NONE',  ( 4.999999999999998224, -42.92893218813448897, -96.95000000000000284 ) ) ;
#7267 = CARTESIAN_POINT ( 'NONE',  ( -31.48612741788231517, -48.30000000000001137, -9.383039235653804155 ) ) ;
#7268 = CARTESIAN_POINT ( 'NONE',  ( 8.389419568037416259E-16, -49.56698729999997255, -99.04999999890752349 ) ) ;
#7269 = VECTOR ( 'NONE', #1700, 1000.000000000000000 ) ;
#7270 = LINE ( 'NONE', #7891, #6210 ) ;
#7271 = CARTESIAN_POINT ( 'NONE',  ( -37.59760657776328685, -37.40140427513058796, 3.811716262761598362 ) ) ;
#7272 = CIRCLE ( 'NONE', #7556, 12.49999999999996980 ) ;
#7273 = CARTESIAN_POINT ( 'NONE',  ( 2.071067811865474173, -39.99999999999997158, -96.04300000002184845 ) ) ;
#7274 = CARTESIAN_POINT ( 'NONE',  ( -22.03669253526174998, -31.34999999999999432, 4.057507815433014642 ) ) ;
#7275 = DIRECTION ( 'NONE',  ( -0.000000000000000000, -1.000000000000000000, 0.000000000000000000 ) ) ;
#7276 = CARTESIAN_POINT ( 'NONE',  ( 30.00000000000001421, -44.99999999999995737, -30.00100000000000122 ) ) ;
#7277 = CONICAL_SURFACE ( 'NONE', #6440, 1.610000000000000098, 0.7853981633974652654 ) ;
#7278 = DIRECTION ( 'NONE',  ( 1.000000000000000000, 0.000000000000000000, 0.000000000000000000 ) ) ;
#7279 = VERTEX_POINT ( 'NONE', #5136 ) ;
#7280 = CARTESIAN_POINT ( 'NONE',  ( -30.00000000000000000, -45.00000000000000000, -30.00100000000000122 ) ) ;
#7281 = CARTESIAN_POINT ( 'NONE',  ( -28.51387258211773812, -34.80000000000000426, 9.383039235653802379 ) ) ;
#7282 = CARTESIAN_POINT ( 'NONE',  ( -25.99212434019154472, -42.65140427513058086, 7.988596311142242890 ) ) ;
#7283 = CARTESIAN_POINT ( 'NONE',  ( 3.535533905932736420, -41.46446609406723383, -96.90000000000000568 ) ) ;
#7284 = CARTESIAN_POINT ( 'NONE',  ( -18.00000000000002132, 1.469576158976823947E-15, -29.65000000000000213 ) ) ;
#7285 = CARTESIAN_POINT ( 'NONE',  ( -25.73429323749904185, -34.59859572486944046, -8.488613101951701267 ) ) ;
#7286 = CARTESIAN_POINT ( 'NONE',  ( -36.71751442127229836, -42.00000000000000711, -6.717514421272142044 ) ) ;
#7287 = EDGE_CURVE ( 'NONE', #5592, #196, #2332, .T. ) ;
#7288 = CARTESIAN_POINT ( 'NONE',  ( -41.99999999999981526, 0.000000000000000000, -45.00000000000000000 ) ) ;
#7289 = DIRECTION ( 'NONE',  ( 0.000000000000000000, 0.000000000000000000, 1.000000000000000000 ) ) ;
#7290 = CARTESIAN_POINT ( 'NONE',  ( -1.891708078845683483, -49.56698729999997255, -100.0999999989075206 ) ) ;
#7291 =( LENGTH_UNIT ( ) NAMED_UNIT ( * ) SI_UNIT ( .MILLI., .METRE. ) );
#7292 = ORIENTED_EDGE ( 'NONE', *, *, #5691, .F. ) ;
#7293 = DIRECTION ( 'NONE',  ( 0.000000000000000000, 1.000000000000000000, -0.000000000000000000 ) ) ;
#7294 = CARTESIAN_POINT ( 'NONE',  ( -23.95213185889994989, -50.49859572486944614, 5.972947139071243861 ) ) ;
#7295 = CARTESIAN_POINT ( 'NONE',  ( -20.12537475255788522, -30.05140427513057944, -1.507589171976365439 ) ) ;
#7296 = EDGE_LOOP ( 'NONE', ( #7920, #2913, #7516, #2071 ) ) ;
#7297 = ORIENTED_EDGE ( 'NONE', *, *, #1884, .T. ) ;
#7298 = CARTESIAN_POINT ( 'NONE',  ( -38.87487832006816291, -49.85140427513058370, -4.584493831696867971 ) ) ;
#7299 = DIRECTION ( 'NONE',  ( -1.000000000000000000, 0.000000000000000000, 0.000000000000000000 ) ) ;
#7300 = CARTESIAN_POINT ( 'NONE',  ( -41.99999999999996447, 48.00000000000002842, 22.00000000000000000 ) ) ;
#7301 = CARTESIAN_POINT ( 'NONE',  ( -2.071067811865475061, -39.99999999999997158, -100.6499999978150441 ) ) ;
#7302 = CARTESIAN_POINT ( 'NONE',  ( 34.74044648917334399, -46.62311395930098712, 11.56703930231303978 ) ) ;
#7303 = CARTESIAN_POINT ( 'NONE',  ( 0.000000000000000000, 0.000000000000000000, 1.622657008870242981E-16 ) ) ;
#7304 = ADVANCED_FACE ( 'NONE', ( #8370 ), #331, .T. ) ;
#7305 = ORIENTED_EDGE ( 'NONE', *, *, #8599, .T. ) ;
#7306 = CARTESIAN_POINT ( 'NONE',  ( -31.32969295284206979, -42.30000000000000426, -8.395350895058669494 ) ) ;
#7307 = ORIENTED_EDGE ( 'NONE', *, *, #3215, .F. ) ;
#7308 = DIRECTION ( 'NONE',  ( -1.000000000000000000, 0.000000000000000000, 0.000000000000000000 ) ) ;
#7309 = CARTESIAN_POINT ( 'NONE',  ( 2.071067811865474173, -39.99999999999997158, -95.94999999781504130 ) ) ;
#7310 = CARTESIAN_POINT ( 'NONE',  ( -34.31290974752564438, -47.10000000000000142, 8.464561979789547053 ) ) ;
#7311 = CARTESIAN_POINT ( 'NONE',  ( -1.891708078845683039, -40.43301269999998482, -99.39999999890751781 ) ) ;
#7312 = CARTESIAN_POINT ( 'NONE',  ( 42.00000000000000711, 47.00857997860455129, -21.99999999999992184 ) ) ;
#7313 = ADVANCED_FACE ( 'NONE', ( #7161 ), #46, .F. ) ;
#7314 = CARTESIAN_POINT ( 'NONE',  ( -33.90612223281073057, -31.10140427513058370, 7.549504333439023718 ) ) ;
#7315 = CONICAL_SURFACE ( 'NONE', #7180, 1.649999999999998579, 1.029744258676653645 ) ;
#7316 = EDGE_CURVE ( 'NONE', #1907, #4613, #3037, .T. ) ;
#7317 = CARTESIAN_POINT ( 'NONE',  ( 4.999999999999998224, -42.92893218813448897, -95.34300000002184561 ) ) ;
#7318 = AXIS2_PLACEMENT_3D ( 'NONE', #1379, #7244, #1916 ) ;
#7319 =( BOUNDED_CURVE ( )  B_SPLINE_CURVE ( 2, ( #2298, #4315, #1579, #3531, #1670, #4361, #4980, #2387, #7043 ),
 .UNSPECIFIED., .F., .T. ) 
 B_SPLINE_CURVE_WITH_KNOTS ( ( 3, 2, 2, 2, 3 ),
 ( 0.4285714285714284366, 0.4464285714285713413, 0.4642857142857141906, 0.4821428571428570953, 0.4999999999999999445 ),
 .UNSPECIFIED. ) 
 CURVE ( )  GEOMETRIC_REPRESENTATION_ITEM ( )  RATIONAL_B_SPLINE_CURVE ( ( 1.000000000000000444, 0.9238795325112862944, 1.000000000000000000, 0.9238795325112867385, 1.000000000000000000, 0.9238795325112867385, 1.000000000000000000, 0.9238795325112869605, 0.9999999999999997780 ) ) 
 REPRESENTATION_ITEM ( '' )  );
#7320 = CARTESIAN_POINT ( 'NONE',  ( -28.67030704715798350, -34.80000000000000426, 8.395350895058669494 ) ) ;
#7321 = DIRECTION ( 'NONE',  ( 1.000000000000000000, 0.000000000000000000, 0.000000000000000000 ) ) ;
#7322 = CARTESIAN_POINT ( 'NONE',  ( -31.56260684030781505, -46.94999999999999574, 9.865911304835508489 ) ) ;
#7323 = ORIENTED_EDGE ( 'NONE', *, *, #2930, .F. ) ;
#7324 = FACE_OUTER_BOUND ( 'NONE', #6676, .T. ) ;
#7325 = CARTESIAN_POINT ( 'NONE',  ( -38.46456197978948666, -47.40000000000001279, 4.312909747525784709 ) ) ;
#7326 = CARTESIAN_POINT ( 'NONE',  ( -22.40239342223677355, -44.90140427513058086, -3.811716262761597473 ) ) ;
#7327 = FACE_BOUND ( 'NONE', #48, .T. ) ;
#7328 = AXIS2_PLACEMENT_3D ( 'NONE', #469, #4585, #3882 ) ;
#7329 = CARTESIAN_POINT ( 'NONE',  ( 34.74126035407623192, -43.37909215248186712, 11.56670877700489264 ) ) ;
#7330 = CARTESIAN_POINT ( 'NONE',  ( -20.14280263777121149, -35.04859572486943620, -1.617624508639600833 ) ) ;
#7331 = DIRECTION ( 'NONE',  ( 0.000000000000000000, 0.000000000000000000, 1.000000000000000000 ) ) ;
#7332 = EDGE_CURVE ( 'NONE', #6167, #7794, #3119, .T. ) ;
#7333 = CYLINDRICAL_SURFACE ( 'NONE', #4986, 1.649999999999998579 ) ;
#7334 = CARTESIAN_POINT ( 'NONE',  ( -2.796473189345805913E-16, -40.43301269999997061, -95.44999999890752918 ) ) ;
#7335 = ORIENTED_EDGE ( 'NONE', *, *, #8697, .F. ) ;
#7336 = DIRECTION ( 'NONE',  ( 0.000000000000000000, 0.000000000000000000, 1.000000000000000000 ) ) ;
#7337 = CARTESIAN_POINT ( 'NONE',  ( -37.57355545560112375, -50.40000000000000568, 3.858919247786223305 ) ) ;
#7338 = CARTESIAN_POINT ( 'NONE',  ( -20.60867331244750034, -32.19859572486942767, 1.433802505903951419 ) ) ;
#7339 = CARTESIAN_POINT ( 'NONE',  ( -31.43380250590416125, -41.30140427513058654, -9.391326687552492558 ) ) ;
#7340 = MECHANICAL_DESIGN_GEOMETRIC_PRESENTATION_REPRESENTATION (  '', ( #2427 ), #5791 ) ;
#7341 = ORIENTED_EDGE ( 'NONE', *, *, #8287, .F. ) ;
#7342 = ORIENTED_EDGE ( 'NONE', *, *, #4705, .F. ) ;
#7343 = CARTESIAN_POINT ( 'NONE',  ( -25.51477047955235378, -48.65140427513057375, 8.925456012876139766 ) ) ;
#7344 = CARTESIAN_POINT ( 'NONE',  ( 2.000000000000000000, 1.773042676681340968, -1.951563910473907981E-15 ) ) ;
#7345 = CARTESIAN_POINT ( 'NONE',  ( -49.99999999999997158, 60.00000000000002842, 30.00000000000000000 ) ) ;
#7346 = CARTESIAN_POINT ( 'NONE',  ( 9.184850993605145972E-16, -49.99999999999997158, -100.2999999978150498 ) ) ;
#7347 = ADVANCED_FACE ( 'NONE', ( #1756 ), #8493, .T. ) ;
#7348 = CARTESIAN_POINT ( 'NONE',  ( -3.061616997868382155E-16, -39.99999999999997158, -95.20000000000000284 ) ) ;
#7349 = CARTESIAN_POINT ( 'NONE',  ( -2.071067811865475061, -39.99999999999997158, -98.35000000000000853 ) ) ;
#7350 = EDGE_LOOP ( 'NONE', ( #4321, #6241 ) ) ;
#7351 = CARTESIAN_POINT ( 'NONE',  ( -25.94249218456686279, -46.65000000000001279, 7.963307464738195840 ) ) ;
#7352 = DIRECTION ( 'NONE',  ( -0.000000000000000000, -0.000000000000000000, -1.000000000000000000 ) ) ;
#7353 = AXIS2_PLACEMENT_3D ( 'NONE', #8173, #4816, #1461 ) ;
#7354 = ADVANCED_FACE ( 'NONE', ( #5754 ), #5094, .F. ) ;
#7355 = CARTESIAN_POINT ( 'NONE',  ( 2.000000000000000000, 1.773042676681340968, -1.951563910473907981E-15 ) ) ;
#7356 = CARTESIAN_POINT ( 'NONE',  ( 1.891708078845682595, -40.43301269999998482, -96.49999999890755475 ) ) ;
#7357 = CARTESIAN_POINT ( 'NONE',  ( 9.184850993605145972E-16, -49.99999999999997158, -96.29999999781504982 ) ) ;
#7358 = CARTESIAN_POINT ( 'NONE',  ( -21.53543802021056663, -42.90000000000000568, -4.312909747525783821 ) ) ;
#7359 = CARTESIAN_POINT ( 'NONE',  ( -3.229347689422840784, -41.77065231057713390, -96.94999999890751496 ) ) ;
#7360 = AXIS2_PLACEMENT_3D ( 'NONE', #1590, #6920, #5032 ) ;
#7361 = VECTOR ( 'NONE', #5061, 1000.000000000000000 ) ;
#7362 = CARTESIAN_POINT ( 'NONE',  ( -35.97294713907137975, -32.00140427513057517, -6.047868141099968398 ) ) ;
#7363 = AXIS2_PLACEMENT_3D ( 'NONE', #2674, #16, #8096 ) ;
#7364 = CARTESIAN_POINT ( 'NONE',  ( 4.999999999999998224, -44.99999999999997158, -96.19300000002185413 ) ) ;
#7365 = CARTESIAN_POINT ( 'NONE',  ( -36.01040764008574513, -36.00000000000000711, -6.010407640085605685 ) ) ;
#7366 = CARTESIAN_POINT ( 'NONE',  ( -40.00000000000002842, 1.224646799147353059E-15, -41.34999999999999432 ) ) ;
#7367 = CARTESIAN_POINT ( 'NONE',  ( 2.000000000000000000, 1.773042676681340968, -1.951563910473907981E-15 ) ) ;
#7368 = DIRECTION ( 'NONE',  ( 1.000000000000000000, 0.000000000000000000, 0.000000000000000000 ) ) ;
#7369 = ORIENTED_EDGE ( 'NONE', *, *, #7175, .F. ) ;
#7370 = CARTESIAN_POINT ( 'NONE',  ( 5.000000000000000000, -47.07106781186545419, -99.45000000000000284 ) ) ;
#7371 = CARTESIAN_POINT ( 'NONE',  ( -25.68709025247441602, -45.60000000000000853, -8.464561979789547053 ) ) ;
#7372 = CARTESIAN_POINT ( 'NONE',  ( -36.31971658582311591, -32.25000000000000711, 6.319716585823199395 ) ) ;
#7373 = SHAPE_REPRESENTATION ( 'shock absorber', ( #2554 ), #2987 ) ;
#7374 = EDGE_CURVE ( 'NONE', #3127, #8141, #2671, .T. ) ;
#7375 = AXIS2_PLACEMENT_3D ( 'NONE', #447, #6454, #8453 ) ;
#7376 = CARTESIAN_POINT ( 'NONE',  ( 4.999999999999998224, -44.99999999999997158, -97.00000000000000000 ) ) ;
#7377 = CARTESIAN_POINT ( 'NONE',  ( -49.99999999999997158, 60.00000000000002842, -30.00000000000000000 ) ) ;
#7378 = CARTESIAN_POINT ( 'NONE',  ( -39.39132668755255651, -45.69859572486943478, -1.433802505903950308 ) ) ;
#7379 = DIRECTION ( 'NONE',  ( 0.000000000000000000, -1.000000000000000000, 0.000000000000000000 ) ) ;
#7380 = DIRECTION ( 'NONE',  ( 0.000000000000000000, 0.000000000000000000, -1.000000000000000000 ) ) ;
#7381 = CARTESIAN_POINT ( 'NONE',  ( -3.229347689422840784, -41.77065231057713390, -96.14999999890753202 ) ) ;
#7382 = VERTEX_POINT ( 'NONE', #6579 ) ;
#7383 = CARTESIAN_POINT ( 'NONE',  ( 0.1999999999999987899, 0.000000000000000000, 3.299999999999999822 ) ) ;
#7384 = CARTESIAN_POINT ( 'NONE',  ( -28.61798213517984024, -32.79859572486943620, 8.387063443159973986 ) ) ;
#7385 = CARTESIAN_POINT ( 'NONE',  ( -25.41550616830297571, -41.64859572486943762, 8.874878320068054549 ) ) ;
#7386 = CARTESIAN_POINT ( 'NONE',  ( -28.56619749409589204, -39.80140427513057944, 9.391326687552490782 ) ) ;
#7387 = ORIENTED_EDGE ( 'NONE', *, *, #7985, .T. ) ;
#7388 = ORIENTED_EDGE ( 'NONE', *, *, #3900, .F. ) ;
#7389 = CARTESIAN_POINT ( 'NONE',  ( -21.51138689804841420, -41.90140427513058086, -4.265706762501151772 ) ) ;
#7390 = PRESENTATION_STYLE_ASSIGNMENT (( #6631 ) ) ;
#7391 = DIRECTION ( 'NONE',  ( 0.000000000000000000, 1.000000000000000000, -8.560894001270036306E-16 ) ) ;
#7392 = CARTESIAN_POINT ( 'NONE',  ( -3.535533905932736864, -41.46446609406723383, -100.5999999978150470 ) ) ;
#7393 = CARTESIAN_POINT ( 'NONE',  ( 33.30764627618177798, -48.76359959685379408, 12.05680772549332680 ) ) ;
#7394 = FACE_OUTER_BOUND ( 'NONE', #3904, .T. ) ;
#7395 = ORIENTED_EDGE ( 'NONE', *, *, #1071, .T. ) ;
#7396 = CARTESIAN_POINT ( 'NONE',  ( -36.04786814110010340, -33.99859572486943904, -5.972947139071243861 ) ) ;
#7397 = CARTESIAN_POINT ( 'NONE',  ( -25.46513832392765408, -37.65000000000000568, 8.900167166472096270 ) ) ;
#7398 = AXIS2_PLACEMENT_3D ( 'NONE', #3657, #7711, #829 ) ;
#7399 = ORIENTED_EDGE ( 'NONE', *, *, #2574, .F. ) ;
#7400 = CARTESIAN_POINT ( 'NONE',  ( -4.566987299999997418, -46.89170807884566017, -96.99999999890751212 ) ) ;
#7401 = CARTESIAN_POINT ( 'NONE',  ( -3.061616997868382155E-16, -39.99999999999997158, -97.49999999781503845 ) ) ;
#7402 = CARTESIAN_POINT ( 'NONE',  ( -39.86591130483550671, -41.55000000000001137, 1.562606840307984468 ) ) ;
#7403 = CARTESIAN_POINT ( 'NONE',  ( 4.566987299999998307, -43.10829192115428299, -99.59999999890756328 ) ) ;
#7404 = APPLICATION_CONTEXT ( 'automotive_design' ) ;
#7405 = CONICAL_SURFACE ( 'NONE', #4732, 2.099999999999997868, 1.029744258676652313 ) ;
#7406 = CARTESIAN_POINT ( 'NONE',  ( -37.93801861833426159, -46.85140427513056949, -4.107139971057695682 ) ) ;
#7407 = CARTESIAN_POINT ( 'NONE',  ( -3.535533905932736864, -41.46446609406723383, -95.09300000002185982 ) ) ;
#7408 = CARTESIAN_POINT ( 'NONE',  ( -33.85891924778610473, -41.10000000000000142, 7.573555455601171715 ) ) ;
#7409 = CARTESIAN_POINT ( 'NONE',  ( -30.00000000000002842, 0.000000000000000000, -44.00000000000000000 ) ) ;
#7410 = CARTESIAN_POINT ( 'NONE',  ( 4.999999999999987566, -42.92893218813447476, -96.04999999781503561 ) ) ;
#7411 = EDGE_CURVE ( 'NONE', #3121, #3466, #6258, .T. ) ;
#7412 = APPLICATION_PROTOCOL_DEFINITION ( 'draft international standard', 'automotive_design', 1998, #2293 ) ;
#7413 = VERTEX_POINT ( 'NONE', #3293 ) ;
#7414 = PLANE ( 'NONE',  #6564 ) ;
#7415 = CARTESIAN_POINT ( 'NONE',  ( -36.71751442127229836, -48.00000000000000711, -6.717514421272142044 ) ) ;
#7416 = CARTESIAN_POINT ( 'NONE',  ( -37.93801861833426159, -46.85140427513056949, -4.107139971057695682 ) ) ;
#7417 = AXIS2_PLACEMENT_3D ( 'NONE', #2945, #4792, #2155 ) ;
#7418 = CARTESIAN_POINT ( 'NONE',  ( -3.535533905932736864, -41.46446609406723383, -96.70000000000000284 ) ) ;
#7419 = ADVANCED_FACE ( 'NONE', ( #3902 ), #1834, .F. ) ;
#7420 = VECTOR ( 'NONE', #2089, 1000.000000000000000 ) ;
#7421 = DIRECTION ( 'NONE',  ( -0.000000000000000000, -0.000000000000000000, 1.000000000000000000 ) ) ;
#7422 = CARTESIAN_POINT ( 'NONE',  ( -36.75497492228666374, -42.99859572486943904, -6.680053920257780220 ) ) ;
#7423 = DIRECTION ( 'NONE',  ( 1.000000000000000000, 0.000000000000000000, 0.000000000000000000 ) ) ;
#7424 = CARTESIAN_POINT ( 'NONE',  ( -23.28248557872775137, -31.50000000000000711, 6.717514421272141156 ) ) ;
#7425 = ORIENTED_EDGE ( 'NONE', *, *, #7917, .T. ) ;
#7426 = DIRECTION ( 'NONE',  ( 0.000000000000000000, 0.4999999999999989453, -0.8660254037844392627 ) ) ;
#7427 = CARTESIAN_POINT ( 'NONE',  ( -31.39812190974910422, -46.94999999999998863, 8.827394325379140483 ) ) ;
#7428 = CARTESIAN_POINT ( 'NONE',  ( -37.02382435302582309, -39.24859572486943904, 7.102600956461226467 ) ) ;
#7429 = CARTESIAN_POINT ( 'NONE',  ( -25.51477047955235378, -45.65140427513058086, 8.925456012876139766 ) ) ;
#7430 = ORIENTED_EDGE ( 'NONE', *, *, #5462, .F. ) ;
#7431 = CIRCLE ( 'NONE', #8147, 0.2000000000000000944 ) ;
#7432 = ORIENTED_EDGE ( 'NONE', *, *, #8448, .F. ) ;
#7433 = CARTESIAN_POINT ( 'NONE',  ( -36.68005392025794009, -41.00140427513057517, -6.754974922286504757 ) ) ;
#7434 = CYLINDRICAL_SURFACE ( 'NONE', #6936, 2.149999999999985256 ) ;
#7435 = DIRECTION ( 'NONE',  ( 0.000000000000000000, 0.000000000000000000, 1.000000000000000000 ) ) ;
#7436 = CARTESIAN_POINT ( 'NONE',  ( -1.891708078845683039, -40.43301269999998482, -95.59999999890753486 ) ) ;
#7437 = DIRECTION ( 'NONE',  ( 0.000000000000000000, -1.000000000000000000, 0.000000000000000000 ) ) ;
#7438 = CARTESIAN_POINT ( 'NONE',  ( -2.071067811865475505, -49.99999999999997158, -96.34999999781506119 ) ) ;
#7439 = ORIENTED_EDGE ( 'NONE', *, *, #4150, .T. ) ;
#7440 = CARTESIAN_POINT ( 'NONE',  ( -38.39535089505872634, -50.70000000000000995, -1.329692952841885267 ) ) ;
#7441 = CARTESIAN_POINT ( 'NONE',  ( -31.48612741788231517, -33.30000000000000426, -9.383039235653804155 ) ) ;
#7442 = EDGE_LOOP ( 'NONE', ( #1400, #6903, #2688 ) ) ;
#7443 = ORIENTED_EDGE ( 'NONE', *, *, #3113, .T. ) ;
#7444 = CARTESIAN_POINT ( 'NONE',  ( -1.891708078845683039, -40.43301269999998482, -96.39999999890753202 ) ) ;
#7445 = CARTESIAN_POINT ( 'NONE',  ( 9.184850993605145972E-16, -49.99999999999997158, -99.59999999999999432 ) ) ;
#7446 = CARTESIAN_POINT ( 'NONE',  ( -28.43739315969223824, -45.45000000000000995, -9.865911304835512041 ) ) ;
#7447 = CARTESIAN_POINT ( 'NONE',  ( -4.566987299999997418, -46.89170807884566727, -97.59999999890756328 ) ) ;
#7448 = EDGE_CURVE ( 'NONE', #772, #8337, #4516, .T. ) ;
#7449 = DIRECTION ( 'NONE',  ( -0.000000000000000000, -0.000000000000000000, -1.000000000000000000 ) ) ;
#7450 = PRODUCT_RELATED_PRODUCT_CATEGORY ( 'part', '', ( #3813 ) ) ;
#7451 = CARTESIAN_POINT ( 'NONE',  ( -37.93801861833426159, -43.85140427513058370, -4.107139971057695682 ) ) ;
#7452 = CARTESIAN_POINT ( 'NONE',  ( -4.999999999999998224, -44.99999999999997158, -97.39300000002185698 ) ) ;
#7453 = CARTESIAN_POINT ( 'NONE',  ( -38.82739432537914581, -44.55000000000000426, 1.398121909749243663 ) ) ;
#7454 = CARTESIAN_POINT ( 'NONE',  ( 26.23319591279775409, -48.30383393989873042, 11.92131216183667597 ) ) ;
#7455 = DIRECTION ( 'NONE',  ( 0.000000000000000000, -0.000000000000000000, -1.000000000000000000 ) ) ;
#7456 = CONTEXT_DEPENDENT_SHAPE_REPRESENTATION ( #2566, #262 ) ;
#7457 = VERTEX_POINT ( 'NONE', #5926 ) ;
#7458 = FACE_BOUND ( 'NONE', #5436, .T. ) ;
#7459 = CARTESIAN_POINT ( 'NONE',  ( -28.43739315969223824, -48.44999999999999574, -9.865911304835512041 ) ) ;
#7460 = CARTESIAN_POINT ( 'NONE',  ( -28.54686042191934092, -47.45140427513057091, -8.818680382772479120 ) ) ;
#7461 = AXIS2_PLACEMENT_3D ( 'NONE', #6354, #5122, #4335 ) ;
#7462 = CARTESIAN_POINT ( 'NONE',  ( -4.999999999999998224, -44.99999999999997158, -95.00000000000000000 ) ) ;
#7463 = CARTESIAN_POINT ( 'NONE',  ( -41.99999999999996447, 48.00000000000002842, 23.64999999999999858 ) ) ;
#7464 = CARTESIAN_POINT ( 'NONE',  ( -25.41550616830297571, -50.64859572486944472, 8.874878320068054549 ) ) ;
#7465 = CARTESIAN_POINT ( 'NONE',  ( 4.200000000000001954, 0.000000000000000000, 0.000000000000000000 ) ) ;
#7466 = DIRECTION ( 'NONE',  ( -0.000000000000000000, 1.000000000000000000, -0.000000000000000000 ) ) ;
#7467 = ORIENTED_EDGE ( 'NONE', *, *, #7961, .T. ) ;
#7468 = CARTESIAN_POINT ( 'NONE',  ( -31.39812190974910422, -49.95000000000000995, 8.827394325379140483 ) ) ;
#7469 = CARTESIAN_POINT ( 'NONE',  ( -37.02382435302582309, -36.24859572486943904, 7.102600956461226467 ) ) ;
#7470 = CARTESIAN_POINT ( 'NONE',  ( -34.36011273255026310, -37.10140427513057659, 8.440510857627391061 ) ) ;
#7471 = AXIS2_PLACEMENT_3D ( 'NONE', #2437, #6965, #7722 ) ;
#7472 = VERTEX_POINT ( 'NONE', #487 ) ;
#7473 = ORIENTED_EDGE ( 'NONE', *, *, #7175, .T. ) ;
#7474 = CARTESIAN_POINT ( 'NONE',  ( -3.229347689422839451, -48.22934768942280925, -97.54999999890752349 ) ) ;
#7475 = PLANE ( 'NONE',  #5817 ) ;
#7476 = CARTESIAN_POINT ( 'NONE',  ( -34.74075059544460231, -43.37701935357448946, 11.56693546130993866 ) ) ;
#7477 = CARTESIAN_POINT ( 'NONE',  ( 2.071067811865474173, -39.99999999999997158, -99.14999999781504414 ) ) ;
#7478 = CARTESIAN_POINT ( 'NONE',  ( -25.64110105645932336, -8.999999999999998224, 124.0000000000000000 ) ) ;
#7479 = DIRECTION ( 'NONE',  ( 0.000000000000000000, 0.000000000000000000, 1.000000000000000000 ) ) ;
#7480 = VERTEX_POINT ( 'NONE', #1917 ) ;
#7481 = CARTESIAN_POINT ( 'NONE',  ( -22.45049566656107842, -34.89859572486943762, -3.906122232810846917 ) ) ;
#7482 = CARTESIAN_POINT ( 'NONE',  ( -31.48612741788231517, -39.30000000000001137, -9.383039235653804155 ) ) ;
#7483 = VERTEX_POINT ( 'NONE', #5177 ) ;
#7484 = AXIS2_PLACEMENT_3D ( 'NONE', #7900, #2527, #1824 ) ;
#7485 = CARTESIAN_POINT ( 'NONE',  ( -49.99999999999997158, -59.99999999999997158, -30.00000000000000000 ) ) ;
#7486 = CARTESIAN_POINT ( 'NONE',  ( 4.566987300000000083, -46.89170807884564596, -96.69999999890751496 ) ) ;
#7487 = CARTESIAN_POINT ( 'NONE',  ( -2.071067811865475061, -39.99999999999997158, -96.64999999781504414 ) ) ;
#7488 = CARTESIAN_POINT ( 'NONE',  ( -38.90016716647221529, -50.84999999999999432, -4.534861676072185155 ) ) ;
#7489 = CARTESIAN_POINT ( 'NONE',  ( -3.229347689422839451, -48.22934768942280925, -99.94999999890752918 ) ) ;
#7490 = AXIS2_PLACEMENT_3D ( 'NONE', #460, #8583, #5852 ) ;
#7492 = CARTESIAN_POINT ( 'NONE',  ( -26.64110105645932336, 10.00000000000000178, -24.00000000000000000 ) ) ;
#7491 = ADVANCED_BREP_SHAPE_REPRESENTATION ( '', ( #3048, #2554 ), #1004 ) ;
#7493 = CARTESIAN_POINT ( 'NONE',  ( -28.54686042191934092, -44.45140427513058512, -8.818680382772479120 ) ) ;
#7494 = AXIS2_PLACEMENT_3D ( 'NONE', #5767, #5023, #1719 ) ;
#7495 = CARTESIAN_POINT ( 'NONE',  ( 4.999999999999998224, -44.99999999999997158, -95.40000000000000568 ) ) ;
#7496 = CARTESIAN_POINT ( 'NONE',  ( -25.94249218456686279, -43.64999999999999858, 7.963307464738194952 ) ) ;
#7497 = CARTESIAN_POINT ( 'NONE',  ( -3.535533905932736864, -41.46446609406723383, -95.79999999781504982 ) ) ;
#7498 = ITEM_DEFINED_TRANSFORMATION ( 'NONE', 'NONE', #430,  #2554 ) ;
#7499 = ORIENTED_EDGE ( 'NONE', *, *, #4668, .F. ) ;
#7500 = CARTESIAN_POINT ( 'NONE',  ( -4.999999999999997335, -47.07106781186546129, -100.4499999978150413 ) ) ;
#7501 = CARTESIAN_POINT ( 'NONE',  ( -39.86591130483550671, -50.55000000000001137, 1.562606840307984468 ) ) ;
#7502 = CARTESIAN_POINT ( 'NONE',  ( -31.27736804086391942, -47.30140427513057944, -8.403638346957361449 ) ) ;
#7503 = CARTESIAN_POINT ( 'NONE',  ( 2.000000000000000000, 0.000000000000000000, 0.000000000000000000 ) ) ;
#7504 = DIRECTION ( 'NONE',  ( -0.7071067811865355823, 8.659560562355079537E-17, -0.7071067811865595631 ) ) ;
#7505 = CARTESIAN_POINT ( 'NONE',  ( -22.97617564697422665, -49.74859572486944614, -7.102600956461224690 ) ) ;
#7506 = CARTESIAN_POINT ( 'NONE',  ( -34.35889894354067309, 8.000000000000000000, 125.0000000000000000 ) ) ;
#7507 = DIRECTION ( 'NONE',  ( -1.000000000000000000, 0.000000000000000000, -0.000000000000000000 ) ) ;
#7508 =( NAMED_UNIT ( * ) SI_UNIT ( $, .STERADIAN. ) SOLID_ANGLE_UNIT ( ) );
#7509 = ORIENTED_EDGE ( 'NONE', *, *, #2395, .T. ) ;
#7510 = CARTESIAN_POINT ( 'NONE',  ( 0.000000000000000000, 0.000000000000000000, 0.000000000000000000 ) ) ;
#7511 = EDGE_LOOP ( 'NONE', ( #7181, #8095 ) ) ;
#7512 = CARTESIAN_POINT ( 'NONE',  ( -22.45049566656107842, -31.89859572486943762, -3.906122232810846917 ) ) ;
#7513 = CARTESIAN_POINT ( 'NONE',  ( -22.97617564697422665, -43.74859572486943904, -7.102600956461224690 ) ) ;
#7514 = CARTESIAN_POINT ( 'NONE',  ( -39.37475178375516549, -37.70140427513057091, -1.538452329860249712 ) ) ;
#7515 = AXIS2_PLACEMENT_3D ( 'NONE', #1206, #1958, #2586 ) ;
#7516 = ORIENTED_EDGE ( 'NONE', *, *, #3878, .T. ) ;
#7517 = CARTESIAN_POINT ( 'NONE',  ( -3.229347689422840784, -41.77065231057713390, -100.1499999989075320 ) ) ;
#7518 = CARTESIAN_POINT ( 'NONE',  ( -20.13408869516453947, -31.05000000000000782, -1.562606840307983136 ) ) ;
#7519 = CARTESIAN_POINT ( 'NONE',  ( -33.30433008846340215, -41.23356742411075260, 12.05770814628969134 ) ) ;
#7520 = CARTESIAN_POINT ( 'NONE',  ( -4.566987299999998307, -44.99999999999997158, -97.04999999890752349 ) ) ;
#7521 = LINE ( 'NONE', #1481, #2175 ) ;
#7522 = CARTESIAN_POINT ( 'NONE',  ( 5.000000000000009770, -47.07106781186543998, -96.14999999781502993 ) ) ;
#7523 = ORIENTED_EDGE ( 'NONE', *, *, #8138, .F. ) ;
#7524 = EDGE_CURVE ( 'NONE', #2150, #1009, #8509, .T. ) ;
#7525 = CARTESIAN_POINT ( 'NONE',  ( -33.81171626276147890, -36.09859572486943335, 7.597606577763319713 ) ) ;
#7526 = CARTESIAN_POINT ( 'NONE',  ( -38.46456197978948666, -35.40000000000000568, 4.312909747525784709 ) ) ;
#7527 = EDGE_LOOP ( 'NONE', ( #3385, #108 ) ) ;
#7528 = CARTESIAN_POINT ( 'NONE',  ( -21.09983283352784156, -49.35000000000000853, 4.534861676072186043 ) ) ;
#7529 = CYLINDRICAL_SURFACE ( 'NONE', #627, 10.00000000000000178 ) ;
#7530 = CARTESIAN_POINT ( 'NONE',  ( 3.535533905932736420, -41.46446609406723383, -98.39999999781504414 ) ) ;
#7531 = DIRECTION ( 'NONE',  ( 1.000000000000000000, 0.000000000000000000, 0.000000000000000000 ) ) ;
#7532 = CARTESIAN_POINT ( 'NONE',  ( 1.891708078845685481, -49.56698729999997255, -98.19999999890751496 ) ) ;
#7533 = CARTESIAN_POINT ( 'NONE',  ( -24.02705286092866643, -42.50140427513057517, 6.047868141099968398 ) ) ;
#7534 = EDGE_CURVE ( 'NONE', #4084, #5699, #5967, .T. ) ;
#7535 = CARTESIAN_POINT ( 'NONE',  ( -3.535533905932735532, -48.53553390593270933, -95.70000000000000284 ) ) ;
#7536 = FACE_OUTER_BOUND ( 'NONE', #7593, .T. ) ;
#7537 = CARTESIAN_POINT ( 'NONE',  ( -21.17260567462091103, -46.05000000000000426, -1.398121909749241887 ) ) ;
#7538 = FACE_OUTER_BOUND ( 'NONE', #3610, .T. ) ;
#7539 = ORIENTED_EDGE ( 'NONE', *, *, #5325, .T. ) ;
#7540 = CARTESIAN_POINT ( 'NONE',  ( 3.535533969928884801, -41.46446615806338087, -100.0000000000000142 ) ) ;
#7541 = FILL_AREA_STYLE_COLOUR ( '', #1593 ) ;
#7542 = CARTESIAN_POINT ( 'NONE',  ( -31.32969295284206979, -39.30000000000001137, -8.395350895058669494 ) ) ;
#7543 = LINE ( 'NONE', #7462, #2054 ) ;
#7544 = AXIS2_PLACEMENT_3D ( 'NONE', #145, #2271, #2843 ) ;
#7545 = LINE ( 'NONE', #6095, #6894 ) ;
#7546 = CARTESIAN_POINT ( 'NONE',  ( -38.92545601287626056, -51.84859572486944757, -4.485229520447501450 ) ) ;
#7547 = DIRECTION ( 'NONE',  ( 0.8660254037844382635, 0.000000000000000000, 0.5000000000000005551 ) ) ;
#7548 = CARTESIAN_POINT ( 'NONE',  ( -38.90016716647221529, -32.85000000000000142, -4.534861676072185155 ) ) ;
#7549 = SHAPE_REPRESENTATION_RELATIONSHIP ( 'NONE' , 'NONE' ,  #3450, #7491 ) ;
#7550 = ORIENTED_EDGE ( 'NONE', *, *, #6788, .F. ) ;
#7551 = CARTESIAN_POINT ( 'NONE',  ( -26.64110105645932336, 8.000000000000000000, -23.99999999999999289 ) ) ;
#7552 = ORIENTED_EDGE ( 'NONE', *, *, #3963, .F. ) ;
#7553 = CARTESIAN_POINT ( 'NONE',  ( -33.81171626276147890, -42.09859572486944046, 7.597606577763319713 ) ) ;
#7554 = CARTESIAN_POINT ( 'NONE',  ( -34.58449383169706692, -46.14859572486944472, -8.874878320068054549 ) ) ;
#7555 = CARTESIAN_POINT ( 'NONE',  ( -31.43380250590416125, -47.30140427513057944, -9.391326687552492558 ) ) ;
#7556 = AXIS2_PLACEMENT_3D ( 'NONE', #529, #620, #5212 ) ;
#7557 = ORIENTED_EDGE ( 'NONE', *, *, #2080, .F. ) ;
#7558 = CARTESIAN_POINT ( 'NONE',  ( -4.566987299999998307, -44.99999999999997158, -96.04999999890752349 ) ) ;
#7559 =( LENGTH_UNIT ( ) NAMED_UNIT ( * ) SI_UNIT ( .MILLI., .METRE. ) );
#7560 = CARTESIAN_POINT ( 'NONE',  ( -34.96646302984643739, -44.33501760501481215, 11.47123432380333341 ) ) ;
#7561 = CARTESIAN_POINT ( 'NONE',  ( -1.891708078845683039, -40.43301269999998482, -98.79999999890753770 ) ) ;
#7562 = LINE ( 'NONE', #4134, #6521 ) ;
#7563 = DIRECTION ( 'NONE',  ( 0.000000000000000000, -1.000000000000000000, 0.000000000000000000 ) ) ;
#7564 = EDGE_LOOP ( 'NONE', ( #6688, #5258, #4166, #5843 ) ) ;
#7565 = VECTOR ( 'NONE', #1905, 1000.000000000000000 ) ;
#7566 = CARTESIAN_POINT ( 'NONE',  ( -21.17260567462091458, -49.04999999999999716, -1.398121909749242331 ) ) ;
#7567 = CARTESIAN_POINT ( 'NONE',  ( -37.06321265474346660, -35.24999999999998579, 7.063212654743582952 ) ) ;
#7568 = ORIENTED_EDGE ( 'NONE', *, *, #2395, .F. ) ;
#7569 = CARTESIAN_POINT ( 'NONE',  ( -38.46456197978948666, -50.40000000000000568, 4.312909747525784709 ) ) ;
#7570 = DIRECTION ( 'NONE',  ( -1.000000000000000000, 0.000000000000000000, 0.000000000000000000 ) ) ;
#7571 = DIRECTION ( 'NONE',  ( 0.000000000000000000, 0.5150380749100549327, 0.8571673007021118895 ) ) ;
#7572 = ADVANCED_FACE ( 'NONE', ( #2626 ), #1332, .T. ) ;
#7573 = CARTESIAN_POINT ( 'NONE',  ( -2.071067811865475061, -39.99999999999997158, -99.04999999781504982 ) ) ;
#7574 = CARTESIAN_POINT ( 'NONE',  ( 3.535533905932737309, -48.53553390593270933, -97.79999999781504982 ) ) ;
#7575 = CARTESIAN_POINT ( 'NONE',  ( 1.891708078845682595, -40.43301269999998482, -99.49999999890754054 ) ) ;
#7576 = EDGE_LOOP ( 'NONE', ( #7658, #4879, #5055, #3817 ) ) ;
#7577 = CARTESIAN_POINT ( 'NONE',  ( -31.45313957808072303, -45.95140427513058512, 8.818680382772479120 ) ) ;
#7578 = PRODUCT_DEFINITION_SHAPE ( 'NONE', 'NONE',  #8731 ) ;
#7579 = CARTESIAN_POINT ( 'NONE',  ( 5.000000000000000000, -47.07106781186545419, -98.64300000002185698 ) ) ;
#7580 = PRODUCT_DEFINITION_CONTEXT ( 'detailed design', #7229, 'design' ) ;
#7581 = CARTESIAN_POINT ( 'NONE',  ( -4.566987299999997418, -46.89170807884566727, -96.79999999890753770 ) ) ;
#7582 = CARTESIAN_POINT ( 'NONE',  ( -36.31971658582311591, -47.25000000000000711, 6.319716585823200283 ) ) ;
#7583 = DIRECTION ( 'NONE',  ( 0.000000000000000000, -1.000000000000000000, 0.000000000000000000 ) ) ;
#7584 = ITEM_DEFINED_TRANSFORMATION ( 'NONE', 'NONE', #1860,  #2554 ) ;
#7585 = CARTESIAN_POINT ( 'NONE',  ( 50.00000000000002842, -30.00000000000000000, 80.00000000000002842 ) ) ;
#7586 = EDGE_CURVE ( 'NONE', #4648, #1297, #3203, .T. ) ;
#7587 = CARTESIAN_POINT ( 'NONE',  ( -22.42644454439892598, -39.90000000000000568, -3.858919247786222861 ) ) ;
#7588 = CARTESIAN_POINT ( 'NONE',  ( 27.92651295580296633, -40.44729329317335242, 12.32776405682970555 ) ) ;
#7589 = DIRECTION ( 'NONE',  ( 0.000000000000000000, 0.5150380749100549327, 0.8571673007021118895 ) ) ;
#7590 = CARTESIAN_POINT ( 'NONE',  ( -34.31290974752564438, -32.10000000000000142, 8.464561979789547053 ) ) ;
#7591 = DIRECTION ( 'NONE',  ( -0.000000000000000000, -0.000000000000000000, -1.000000000000000000 ) ) ;
#7592 = DIRECTION ( 'NONE',  ( 0.000000000000000000, 0.000000000000000000, 1.000000000000000000 ) ) ;
#7593 = EDGE_LOOP ( 'NONE', ( #510, #2118 ) ) ;
#7594 = FACE_BOUND ( 'NONE', #4581, .T. ) ;
#7595 = ORIENTED_EDGE ( 'NONE', *, *, #5163, .F. ) ;
#7596 = CARTESIAN_POINT ( 'NONE',  ( -23.95213185889994989, -35.49859572486943193, 5.972947139071243861 ) ) ;
#7597 = CARTESIAN_POINT ( 'NONE',  ( -38.44051085762733777, -51.39859572486944472, 4.360112732550414982 ) ) ;
#7598 = CARTESIAN_POINT ( 'NONE',  ( -37.10260095646111012, -46.25140427513058228, 7.023824353025939438 ) ) ;
#7599 = AXIS2_PLACEMENT_3D ( 'NONE', #7783, #1163, #1753 ) ;
#7600 = CARTESIAN_POINT ( 'NONE',  ( -2.796473189345805913E-16, -40.43301269999997061, -97.04999999890752349 ) ) ;
#7601 = CARTESIAN_POINT ( 'NONE',  ( -21.09983283352784156, -31.34999999999999787, 4.534861676072186043 ) ) ;
#7602 = DIRECTION ( 'NONE',  ( -0.000000000000000000, 0.000000000000000000, -1.000000000000000000 ) ) ;
#7603 = CIRCLE ( 'NONE', #3247, 11.99999999999983302 ) ;
#7604 = CARTESIAN_POINT ( 'NONE',  ( -1.891708078845683483, -49.56698729999997255, -96.89999999890751781 ) ) ;
#7605 = EDGE_CURVE ( 'NONE', #7164, #3309, #7245, .T. ) ;
#7606 = DIRECTION ( 'NONE',  ( 1.000000000000000000, 0.000000000000000000, -0.000000000000000000 ) ) ;
#7607 = DIRECTION ( 'NONE',  ( 0.000000000000000000, 0.000000000000000000, -1.000000000000000000 ) ) ;
#7608 =( BOUNDED_CURVE ( )  B_SPLINE_CURVE ( 2, ( #3957, #8014, #1971, #4659, #7348, #2686, #5353, #6285, #246 ),
 .UNSPECIFIED., .F., .T. ) 
 B_SPLINE_CURVE_WITH_KNOTS ( ( 3, 2, 2, 2, 3 ),
 ( 0.000000000000000000, 0.01785714285714286309, 0.03571428571428572618, 0.05357142857142858927, 0.07142857142857145236 ),
 .UNSPECIFIED. ) 
 CURVE ( )  GEOMETRIC_REPRESENTATION_ITEM ( )  RATIONAL_B_SPLINE_CURVE ( ( 1.000000000000000000, 0.9238795325112867385, 1.000000000000000000, 0.9238795325112867385, 1.000000000000000000, 0.9238795325112867385, 1.000000000000000000, 0.9238795325112866275, 1.000000000000000222 ) ) 
 REPRESENTATION_ITEM ( '' )  );
#7609 = VERTEX_POINT ( 'NONE', #2537 ) ;
#7610 = CARTESIAN_POINT ( 'NONE',  ( -23.71967171589458445, -37.74859572486943904, -6.359104887540838469 ) ) ;
#7611 = CARTESIAN_POINT ( 'NONE',  ( -25.46513832392765408, -40.65000000000000568, 8.900167166472096270 ) ) ;
#7612 = AXIS2_PLACEMENT_3D ( 'NONE', #349, #3057, #8432 ) ;
#7613 = ORIENTED_EDGE ( 'NONE', *, *, #2526, .F. ) ;
#7614 = CARTESIAN_POINT ( 'NONE',  ( -31.48612741788231517, -45.30000000000000426, -9.383039235653804155 ) ) ;
#7615 = CARTESIAN_POINT ( 'NONE',  ( -2.071067811865475505, -49.99999999999996447, -99.54999999781506403 ) ) ;
#7616 = CARTESIAN_POINT ( 'NONE',  ( -4.999999999999986677, -47.07106781186546129, -98.04999999781503561 ) ) ;
#7617 = CARTESIAN_POINT ( 'NONE',  ( 1.891708078845685481, -49.56698729999997255, -99.79999999890752349 ) ) ;
#7618 = ORIENTED_EDGE ( 'NONE', *, *, #8170, .T. ) ;
#7619 = CARTESIAN_POINT ( 'NONE',  ( -37.59760657776328685, -49.40140427513058086, 3.811716262761598362 ) ) ;
#7620 =( GEOMETRIC_REPRESENTATION_CONTEXT ( 3 ) GLOBAL_UNCERTAINTY_ASSIGNED_CONTEXT ( ( #5641 ) ) GLOBAL_UNIT_ASSIGNED_CONTEXT ( ( #1028, #3154, #5084 ) ) REPRESENTATION_CONTEXT ( 'NONE', 'WORKASPACE' ) );
#7621 = ADVANCED_FACE ( 'NONE', ( #8573 ), #5296, .F. ) ;
#7622 = CARTESIAN_POINT ( 'NONE',  ( -3.061616997868382155E-16, -39.99999999999997158, -99.19300000002183992 ) ) ;
#7623 = DIRECTION ( 'NONE',  ( 1.000000000000000000, 0.000000000000000000, -0.000000000000000000 ) ) ;
#7624 = CARTESIAN_POINT ( 'NONE',  ( -4.999999999999998224, -42.92893218813448897, -96.54999999781504982 ) ) ;
#7625 = CARTESIAN_POINT ( 'NONE',  ( 0.000000000000000000, -0.8865213383406692627, 1.535500000000001641 ) ) ;
#7626 = CONTEXT_DEPENDENT_SHAPE_REPRESENTATION ( #1666, #889 ) ;
#7627 = DIRECTION ( 'NONE',  ( 0.000000000000000000, 0.000000000000000000, 1.000000000000000000 ) ) ;
#7628 = ADVANCED_FACE ( 'NONE', ( #6711 ), #7333, .F. ) ;
#7629 = CARTESIAN_POINT ( 'NONE',  ( -36.01040764008574513, -39.00000000000000711, -6.010407640085605685 ) ) ;
#7630 = AXIS2_PLACEMENT_3D ( 'NONE', #3789, #8383, #342 ) ;
#7631 = CARTESIAN_POINT ( 'NONE',  ( 4.000000000000001776, 2.694222958124178486E-16, 2.200000000000001066 ) ) ;
#7632 = DIRECTION ( 'NONE',  ( 0.000000000000000000, 0.000000000000000000, 1.000000000000000000 ) ) ;
#7633 = CARTESIAN_POINT ( 'NONE',  ( -20.61696076434619584, -34.20000000000000995, 1.486127417882100676 ) ) ;
#7634 = CARTESIAN_POINT ( 'NONE',  ( -3.535533905932735532, -48.53553390593270933, -98.10000000000000853 ) ) ;
#7635 = CARTESIAN_POINT ( 'NONE',  ( -36.71751442127229836, -36.00000000000000711, -6.717514421272142044 ) ) ;
#7636 = VECTOR ( 'NONE', #7191, 1000.000000000000227 ) ;
#7637 = SURFACE_STYLE_FILL_AREA ( #6844 ) ;
#7638 = EDGE_LOOP ( 'NONE', ( #955, #661, #4844, #8101 ) ) ;
#7639 = CARTESIAN_POINT ( 'NONE',  ( 2.000000000000000000, 2.253471898105739434E-15, 1.535500000000000309 ) ) ;
#7640 = ORIENTED_EDGE ( 'NONE', *, *, #6037, .T. ) ;
#7641 = VECTOR ( 'NONE', #5935, 1000.000000000000000 ) ;
#7642 = CARTESIAN_POINT ( 'NONE',  ( -28.61798213517984024, -35.79859572486943620, 8.387063443159973986 ) ) ;
#7643 = CARTESIAN_POINT ( 'NONE',  ( -34.58449383169706692, -49.14859572486945183, -8.874878320068054549 ) ) ;
#7644 = CARTESIAN_POINT ( 'NONE',  ( -24.02705286092866643, -33.50140427513058228, 6.047868141099968398 ) ) ;
#7645 = EDGE_CURVE ( 'NONE', #7609, #1046, #1287, .T. ) ;
#7646 = CARTESIAN_POINT ( 'NONE',  ( -4.566987299999997418, -46.89170807884566017, -97.59999999890754907 ) ) ;
#7647 = PRESENTATION_LAYER_ASSIGNMENT (  '', '', ( #186 ) ) ;
#7648 = CARTESIAN_POINT ( 'NONE',  ( 4.999999999999998224, -44.99999999999997158, -96.89999999781505835 ) ) ;
#7649 = CARTESIAN_POINT ( 'NONE',  ( -34.35889894354067309, -8.999999999999998224, 124.0000000000000000 ) ) ;
#7650 = CARTESIAN_POINT ( 'NONE',  ( 1.891708078845685481, -49.56698729999997255, -99.19999999890751496 ) ) ;
#7651 = CARTESIAN_POINT ( 'NONE',  ( 7.499999999999999112, -44.99999999999997158, -105.0000000000000142 ) ) ;
#7652 = CARTESIAN_POINT ( 'NONE',  ( -1.891708078845683483, -49.56698729999997255, -98.49999999890752633 ) ) ;
#7653 = CYLINDRICAL_SURFACE ( 'NONE', #2695, 4.999999999999998224 ) ;
#7654 = VERTEX_POINT ( 'NONE', #4605 ) ;
#7655 = CARTESIAN_POINT ( 'NONE',  ( -22.45049566656107842, -40.89859572486943762, -3.906122232810846917 ) ) ;
#7656 = VECTOR ( 'NONE', #7437, 1000.000000000000000 ) ;
#7657 = CARTESIAN_POINT ( 'NONE',  ( -20.61696076434619584, -40.20000000000000995, 1.486127417882100676 ) ) ;
#7658 = ORIENTED_EDGE ( 'NONE', *, *, #465, .F. ) ;
#7659 = CARTESIAN_POINT ( 'NONE',  ( -34.53486167607238144, -48.15000000000001279, -8.900167166472096270 ) ) ;
#7660 = CARTESIAN_POINT ( 'NONE',  ( -4.999999999999998224, -44.99999999999997158, -99.69999999781505551 ) ) ;
#7661 = CARTESIAN_POINT ( 'NONE',  ( -3.229347689422840784, -41.77065231057713390, -99.54999999890752349 ) ) ;
#7662 = CONICAL_SURFACE ( 'NONE', #3865, 1.649999999999998579, 1.029744258676653645 ) ;
#7663 = CARTESIAN_POINT ( 'NONE',  ( 2.071067811865474173, -39.99999999999997158, -99.14999999781504414 ) ) ;
#7664 = DIRECTION ( 'NONE',  ( 0.000000000000000000, 0.000000000000000000, 1.000000000000000000 ) ) ;
#7665 = CARTESIAN_POINT ( 'NONE',  ( -3.229347689422839451, -48.22934768942280925, -97.54999999890752349 ) ) ;
#7666 = ORIENTED_EDGE ( 'NONE', *, *, #2574, .T. ) ;
#7667 = CARTESIAN_POINT ( 'NONE',  ( -31.39812190974910422, -31.95000000000000639, 8.827394325379140483 ) ) ;
#7668 = CARTESIAN_POINT ( 'NONE',  ( -4.999999999999998224, -46.91341716182541433, -94.95380602337444031 ) ) ;
#7669 = ADVANCED_FACE ( 'NONE', ( #3332 ), #6009, .F. ) ;
#7670 = CARTESIAN_POINT ( 'NONE',  ( 1.891708078845685481, -49.56698729999997255, -95.79999999890752349 ) ) ;
#7671 = CARTESIAN_POINT ( 'NONE',  ( 2.071067811865474173, -39.99999999999997158, -95.94999999781504130 ) ) ;
#7672 = DIRECTION ( 'NONE',  ( 1.000000000000000000, 0.000000000000000000, 0.000000000000000000 ) ) ;
#7673 = EDGE_CURVE ( 'NONE', #8625, #5629, #2737, .T. ) ;
#7674 = CARTESIAN_POINT ( 'NONE',  ( -4.999999999999998224, -44.99999999999997158, -100.4999999978150385 ) ) ;
#7675 = CARTESIAN_POINT ( 'NONE',  ( -23.68028341417693738, -39.74999999999999289, -6.319716585823198507 ) ) ;
#7676 = PRODUCT ( 'guide block', 'guide block', '', ( #4727 ) ) ;
#7677 = AXIS2_PLACEMENT_3D ( 'NONE', #2045, #3939, #8038 ) ;
#7678 = CARTESIAN_POINT ( 'NONE',  ( -1.891708078845683705, -49.56698729999997255, -96.09999999890752065 ) ) ;
#7679 = CARTESIAN_POINT ( 'NONE',  ( -3.061616997868382155E-16, -39.99999999999997158, -98.40000000000000568 ) ) ;
#7680 = CARTESIAN_POINT ( 'NONE',  ( -31.48612741788231517, -33.30000000000000426, -9.383039235653804155 ) ) ;
#7681 = ADVANCED_FACE ( 'NONE', ( #8042 ), #2003, .F. ) ;
#7682 = DIRECTION ( 'NONE',  ( 0.000000000000000000, 0.000000000000000000, -1.000000000000000000 ) ) ;
#7683 = CARTESIAN_POINT ( 'NONE',  ( -21.09983283352783801, -37.35000000000000853, 4.534861676072186043 ) ) ;
#7684 = APPLICATION_CONTEXT ( 'automotive_design' ) ;
#7685 = CARTESIAN_POINT ( 'NONE',  ( 0.000000000000000000, 0.000000000000000000, 0.000000000000000000 ) ) ;
#7686 = ORIENTED_EDGE ( 'NONE', *, *, #1396, .F. ) ;
#7687 = CARTESIAN_POINT ( 'NONE',  ( -35.35889894354067309, 8.000000000000000000, -25.00000000000000000 ) ) ;
#7688 = ORIENTED_EDGE ( 'NONE', *, *, #515, .F. ) ;
#7689 = CARTESIAN_POINT ( 'NONE',  ( -31.38201786482021305, -43.29859572486943620, -8.387063443159975762 ) ) ;
#7690 = AXIS2_PLACEMENT_3D ( 'NONE', #2967, #1679, #4943 ) ;
#7691 = CARTESIAN_POINT ( 'NONE',  ( -34.26570676250101855, -45.09859572486944046, 8.488613101951703044 ) ) ;
#7692 = CARTESIAN_POINT ( 'NONE',  ( -28.54686042191934092, -32.45140427513058512, -8.818680382772479120 ) ) ;
#7693 = AXIS2_PLACEMENT_3D ( 'NONE', #8142, #2101, #4784 ) ;
#7694 = EDGE_CURVE ( 'NONE', #7212, #8113, #3594, .T. ) ;
#7695 = CARTESIAN_POINT ( 'NONE',  ( -1.891708078845683039, -40.43301269999998482, -98.59999999890754907 ) ) ;
#7696 = CARTESIAN_POINT ( 'NONE',  ( 32.22816283978665552, -40.51193879865773084, 12.30361675895771967 ) ) ;
#7697 = CARTESIAN_POINT ( 'NONE',  ( -30.00000000000000000, 60.00000000000002842, 0.000000000000000000 ) ) ;
#7698 = CIRCLE ( 'NONE', #7255, 2.099999999999997868 ) ;
#7699 = CARTESIAN_POINT ( 'NONE',  ( 1.891708078845682595, -40.43301269999998482, -96.49999999890752633 ) ) ;
#7700 = CARTESIAN_POINT ( 'NONE',  ( 4.566987300000000083, -46.89170807884565306, -96.69999999890752918 ) ) ;
#7701 = EDGE_CURVE ( 'NONE', #6319, #71, #6696, .T. ) ;
#7702 = EDGE_CURVE ( 'NONE', #3069, #6952, #2601, .T. ) ;
#7703 =( NAMED_UNIT ( * ) PLANE_ANGLE_UNIT ( ) SI_UNIT ( $, .RADIAN. ) );
#7704 = ORIENTED_EDGE ( 'NONE', *, *, #6060, .F. ) ;
#7705 = CARTESIAN_POINT ( 'NONE',  ( -37.98859631114233792, -42.84859572486944046, -4.007875659808334490 ) ) ;
#7706 = CARTESIAN_POINT ( 'NONE',  ( -22.93678734525658314, -45.74999999999999289, -7.063212654743582952 ) ) ;
#7707 = CIRCLE ( 'NONE', #5872, 2.099999999999997868 ) ;
#7708 = ORIENTED_EDGE ( 'NONE', *, *, #735, .T. ) ;
#7709 = CARTESIAN_POINT ( 'NONE',  ( -31.61762450863942320, -30.95140427513058157, 9.857197362228843573 ) ) ;
#7710 = CARTESIAN_POINT ( 'NONE',  ( -32.23060284177036294, -49.48683715626712853, 12.30316928347423655 ) ) ;
#7711 = DIRECTION ( 'NONE',  ( -0.000000000000000000, 1.000000000000000000, -0.000000000000000000 ) ) ;
#7712 = CARTESIAN_POINT ( 'NONE',  ( -4.999999999999998224, -44.99999999999997158, -97.29999999781504982 ) ) ;
#7713 = LINE ( 'NONE', #1673, #2569 ) ;
#7714 = AXIS2_PLACEMENT_3D ( 'NONE', #434, #6402, #5828 ) ;
#7715 = CARTESIAN_POINT ( 'NONE',  ( 3.535533905932737309, -48.53553390593270933, -97.90000000000000568 ) ) ;
#7716 = ORIENTED_EDGE ( 'NONE', *, *, #8287, .T. ) ;
#7717 = CARTESIAN_POINT ( 'NONE',  ( -28.67030704715798350, -31.80000000000000782, 8.395350895058669494 ) ) ;
#7718 = ORIENTED_EDGE ( 'NONE', *, *, #2699, .T. ) ;
#7719 = CARTESIAN_POINT ( 'NONE',  ( 2.000000000000000000, 1.773042676681340968, -1.951563910473907981E-15 ) ) ;
#7720 = ADVANCED_FACE ( 'NONE', ( #2760 ), #762, .F. ) ;
#7721 = CARTESIAN_POINT ( 'NONE',  ( -3.535533905932735532, -48.53553390593270933, -97.19999999781504130 ) ) ;
#7722 = DIRECTION ( 'NONE',  ( 1.000000000000000000, 0.000000000000000000, 0.000000000000000000 ) ) ;
#7723 = CONTEXT_DEPENDENT_SHAPE_REPRESENTATION ( #3474, #6245 ) ;
#7724 = DIRECTION ( 'NONE',  ( 0.000000000000000000, 0.000000000000000000, 1.000000000000000000 ) ) ;
#7725 = CARTESIAN_POINT ( 'NONE',  ( -21.60464910494133406, -34.20000000000000995, 1.329692952841886155 ) ) ;
#7726 = PRODUCT_DEFINITION_SHAPE ( 'NONE', 'NONE',  #8724 ) ;
#7727 = CARTESIAN_POINT ( 'NONE',  ( 1.891708078845685481, -49.56698729999997255, -95.99999999890751212 ) ) ;
#7728 = CARTESIAN_POINT ( 'NONE',  ( 45.00000000000003553, -44.99999999999997158, -2.099999999999997868 ) ) ;
#7729 = CARTESIAN_POINT ( 'NONE',  ( -36.71751442127229836, -30.00000000000000711, -6.717514421272142044 ) ) ;
#7730 = LINE ( 'NONE', #8440, #4332 ) ;
#7731 = CARTESIAN_POINT ( 'NONE',  ( -28.51387258211773812, -40.80000000000000426, 9.383039235653802379 ) ) ;
#7732 = ORIENTED_EDGE ( 'NONE', *, *, #3921, .T. ) ;
#7733 = ORIENTED_EDGE ( 'NONE', *, *, #3105, .F. ) ;
#7734 = CARTESIAN_POINT ( 'NONE',  ( -38.40363834695740053, -42.69859572486944188, -1.277368040863739118 ) ) ;
#7735 = CARTESIAN_POINT ( 'NONE',  ( -20.14280263777121149, -47.04859572486944330, -1.617624508639600833 ) ) ;
#7736 = CARTESIAN_POINT ( 'NONE',  ( -37.93801861833426159, -31.85140427513056594, -4.107139971057695682 ) ) ;
#7737 = CARTESIAN_POINT ( 'NONE',  ( 8.389419568037416259E-16, -49.56698729999997255, -98.24999999890752633 ) ) ;
#7738 = UNCERTAINTY_MEASURE_WITH_UNIT (LENGTH_MEASURE( 1.000000000000000082E-05 ), #896, 'distance_accuracy_value', 'NONE');
#7739 = CARTESIAN_POINT ( 'NONE',  ( 50.00000000000002842, 30.00000000000000000, 80.00000000000002842 ) ) ;
#7740 = CARTESIAN_POINT ( 'NONE',  ( -31.56260684030781505, -40.95000000000000995, 9.865911304835510265 ) ) ;
#7741 = CARTESIAN_POINT ( 'NONE',  ( -41.99999999999996447, 22.00000000000000000, 80.00000000000002842 ) ) ;
#7742 = CARTESIAN_POINT ( 'NONE',  ( -28.37754256541759190, -49.74093594125429263, 12.39808714042240645 ) ) ;
#7743 = CARTESIAN_POINT ( 'NONE',  ( 3.229347689422841228, -48.22934768942280925, -95.94999999890751496 ) ) ;
#7744 = AXIS2_PLACEMENT_3D ( 'NONE', #4908, #2757, #806 ) ;
#7745 = EDGE_LOOP ( 'NONE', ( #4265, #2447, #5814, #5940 ) ) ;
#7746 = CARTESIAN_POINT ( 'NONE',  ( -31.34310424141748896, -44.94859572486942767, 8.836108267985801845 ) ) ;
#7747 = CARTESIAN_POINT ( 'NONE',  ( -36.71751442127229836, -48.00000000000000711, -6.717514421272142044 ) ) ;
#7748 = ORIENTED_EDGE ( 'NONE', *, *, #7287, .T. ) ;
#7749 = CARTESIAN_POINT ( 'NONE',  ( -37.10260095646111012, -40.25140427513058228, 7.023824353025939438 ) ) ;
#7750 = CIRCLE ( 'NONE', #844, 1.610000000000000098 ) ;
#7751 = CYLINDRICAL_SURFACE ( 'NONE', #7852, 4.999999999999998224 ) ;
#7752 = FACE_OUTER_BOUND ( 'NONE', #4276, .T. ) ;
#7753 = CARTESIAN_POINT ( 'NONE',  ( -2.071067811865475505, -49.99999999999997158, -95.65000000000000568 ) ) ;
#7754 = FACE_OUTER_BOUND ( 'NONE', #7576, .T. ) ;
#7755 = CARTESIAN_POINT ( 'NONE',  ( 2.071067811865477282, -49.99999999999996447, -97.95000000000000284 ) ) ;
#7756 = ORIENTED_EDGE ( 'NONE', *, *, #886, .T. ) ;
#7757 = PRODUCT_DEFINITION_SHAPE ( 'NONE', 'NONE',  #8720 ) ;
#7758 = CARTESIAN_POINT ( 'NONE',  ( -36.31971658582311591, -35.24999999999998579, 6.319716585823199395 ) ) ;
#7759 = VECTOR ( 'NONE', #5757, 1000.000000000000000 ) ;
#7760 = VERTEX_POINT ( 'NONE', #2144 ) ;
#7761 = CARTESIAN_POINT ( 'NONE',  ( -4.999999999999998224, -42.92893218813448897, -98.25000000000000000 ) ) ;
#7762 = CARTESIAN_POINT ( 'NONE',  ( 4.999999999999998224, -44.99999999999997158, -96.89999999781505835 ) ) ;
#7763 = DIRECTION ( 'NONE',  ( 0.000000000000000000, 1.000000000000000000, -1.467581828789149335E-15 ) ) ;
#7764 = CARTESIAN_POINT ( 'NONE',  ( -34.35889894354067309, -8.999999999999998224, 125.0000000000000000 ) ) ;
#7765 = CARTESIAN_POINT ( 'NONE',  ( -37.96330746473829976, -44.85000000000001563, -4.057507815433013754 ) ) ;
#7766 = DIRECTION ( 'NONE',  ( 1.000000000000000000, -0.000000000000000000, -0.000000000000000000 ) ) ;
#7767 = DIRECTION ( 'NONE',  ( -0.000000000000000000, -0.000000000000000000, -1.000000000000000000 ) ) ;
#7768 = CARTESIAN_POINT ( 'NONE',  ( -21.53543802021056663, -36.90000000000000568, -4.312909747525783821 ) ) ;
#7769 = DIRECTION ( 'NONE',  ( -0.000000000000000000, -0.000000000000000000, 1.000000000000000000 ) ) ;
#7770 = CARTESIAN_POINT ( 'NONE',  ( -37.06321265474346660, -38.25000000000001421, 7.063212654743582952 ) ) ;
#7771 = CARTESIAN_POINT ( 'NONE',  ( 2.000000000000000000, 0.8865213383406683745, -1.535500000000000753 ) ) ;
#7772 = CARTESIAN_POINT ( 'NONE',  ( -20.61696076434619584, -40.20000000000000995, 1.486127417882100676 ) ) ;
#7773 = FILL_AREA_STYLE ('',( #2980 ) ) ;
#7774 = ORIENTED_EDGE ( 'NONE', *, *, #786, .T. ) ;
#7775 = CARTESIAN_POINT ( 'NONE',  ( -28.65689575858256077, -49.44859572486943478, -8.836108267985801845 ) ) ;
#7776 = CARTESIAN_POINT ( 'NONE',  ( -23.28248557872775137, -37.50000000000000711, 6.717514421272141156 ) ) ;
#7777 = CIRCLE ( 'NONE', #6925, 12.00000000000000000 ) ;
#7778 = CARTESIAN_POINT ( 'NONE',  ( -22.06198138166579170, -39.35140427513057659, 4.107139971057695682 ) ) ;
#7779 = CARTESIAN_POINT ( 'NONE',  ( -1.891708078845683039, -40.43301269999998482, -99.39999999890751781 ) ) ;
#7780 = CARTESIAN_POINT ( 'NONE',  ( 44.14999999999999147, -21.99999999999992184, 80.00000000000002842 ) ) ;
#7781 = CARTESIAN_POINT ( 'NONE',  ( -37.06321265474346660, -41.25000000000000711, 7.063212654743582952 ) ) ;
#7782 = CIRCLE ( 'NONE', #3981, 10.00000000000000000 ) ;
#7783 = CARTESIAN_POINT ( 'NONE',  ( 0.000000000000000000, -44.99999999999997158, -105.0000000000000142 ) ) ;
#7784 = CYLINDRICAL_SURFACE ( 'NONE', #4279, 10.00000000000000178 ) ;
#7785 = CIRCLE ( 'NONE', #2440, 12.65000000000000036 ) ;
#7786 = CARTESIAN_POINT ( 'NONE',  ( -3.229347689422840784, -41.77065231057713390, -97.14999999890753202 ) ) ;
#7787 = CARTESIAN_POINT ( 'NONE',  ( 0.000000000000000000, 0.000000000000000000, 0.000000000000000000 ) ) ;
#7788 = ORIENTED_EDGE ( 'NONE', *, *, #5099, .F. ) ;
#7789 = SURFACE_STYLE_FILL_AREA ( #4198 ) ;
#7790 = CARTESIAN_POINT ( 'NONE',  ( -28.61798213517984024, -41.79859572486943620, 8.387063443159973986 ) ) ;
#7791 = CARTESIAN_POINT ( 'NONE',  ( -22.93678734525658314, -48.75000000000001421, -7.063212654743582952 ) ) ;
#7792 = EDGE_CURVE ( 'NONE', #282, #7915, #676, .T. ) ;
#7793 = AXIS2_PLACEMENT_3D ( 'NONE', #7510, #6100, #4123 ) ;
#7794 = VERTEX_POINT ( 'NONE', #5165 ) ;
#7795 = CARTESIAN_POINT ( 'NONE',  ( -34.48522952044771017, -32.15140427513058086, -8.925456012876139766 ) ) ;
#7796 = DIRECTION ( 'NONE',  ( -0.000000000000000000, -0.000000000000000000, -1.000000000000000000 ) ) ;
#7797 = DIRECTION ( 'NONE',  ( 0.000000000000000000, 0.000000000000000000, -1.000000000000000000 ) ) ;
#7798 = DIRECTION ( 'NONE',  ( -0.000000000000000000, -0.000000000000000000, -1.000000000000000000 ) ) ;
#7799 = CARTESIAN_POINT ( 'NONE',  ( -30.00000000000002842, 0.000000000000000000, -28.65000000000000213 ) ) ;
#7800 = CARTESIAN_POINT ( 'NONE',  ( 4.999999999999998224, -44.99999999999997158, -96.20000000000000284 ) ) ;
#7801 = ADVANCED_FACE ( 'NONE', ( #3844 ), #2661, .F. ) ;
#7802 = ORIENTED_EDGE ( 'NONE', *, *, #6398, .T. ) ;
#7803 = CARTESIAN_POINT ( 'NONE',  ( -28.60187809025093841, -36.45000000000000284, -8.827394325379140483 ) ) ;
#7804 = AXIS2_PLACEMENT_3D ( 'NONE', #730, #3437, #6112 ) ;
#7805 = EDGE_CURVE ( 'NONE', #5614, #4623, #6568, .T. ) ;
#7806 = ORIENTED_EDGE ( 'NONE', *, *, #2361, .F. ) ;
#7807 = CARTESIAN_POINT ( 'NONE',  ( -4.999999999999998224, -44.99999999999997158, -99.00000000000000000 ) ) ;
#7808 = ADVANCED_BREP_SHAPE_REPRESENTATION ( '', ( #5903, #2554 ), #2987 ) ;
#7809 = CARTESIAN_POINT ( 'NONE',  ( 3.535533905932737309, -48.53553390593270933, -96.99999999781503845 ) ) ;
#7810 = CARTESIAN_POINT ( 'NONE',  ( -3.570038910208443106, -48.51199280350586207, -100.0000267679173760 ) ) ;
#7811 = EDGE_CURVE ( 'NONE', #3910, #1209, #1948, .T. ) ;
#7812 = FACE_OUTER_BOUND ( 'NONE', #634, .T. ) ;
#7813 = DIRECTION ( 'NONE',  ( 0.000000000000000000, -0.4999999999999989453, 0.8660254037844391517 ) ) ;
#7814 = EDGE_CURVE ( 'NONE', #8507, #2302, #5815, .T. ) ;
#7815 = CARTESIAN_POINT ( 'NONE',  ( 2.000000000000000000, 1.773042676681340968, -1.951563910473907981E-15 ) ) ;
#7816 = CYLINDRICAL_SURFACE ( 'NONE', #7990, 4.999999999999998224 ) ;
#7817 = CARTESIAN_POINT ( 'NONE',  ( -28.51387258211773812, -37.80000000000000426, 9.383039235653802379 ) ) ;
#7818 = DIRECTION ( 'NONE',  ( 1.000000000000000000, 0.000000000000000000, 0.000000000000000000 ) ) ;
#7819 = ORIENTED_EDGE ( 'NONE', *, *, #1421, .T. ) ;
#7820 = CARTESIAN_POINT ( 'NONE',  ( -33.81171626276147890, -51.09859572486944046, 7.597606577763319713 ) ) ;
#7821 = CARTESIAN_POINT ( 'NONE',  ( -20.61696076434619584, -40.20000000000000995, 1.486127417882100676 ) ) ;
#7822 = CARTESIAN_POINT ( 'NONE',  ( -35.97294713907137975, -38.00140427513057517, -6.047868141099968398 ) ) ;
#7823 = CIRCLE ( 'NONE', #1776, 11.99999999999979217 ) ;
#7824 = CARTESIAN_POINT ( 'NONE',  ( 3.229347689422839895, -41.77065231057713390, -99.54999999890752349 ) ) ;
#7825 = PLANE ( 'NONE',  #6851 ) ;
#7826 = CARTESIAN_POINT ( 'NONE',  ( -38.46456197978948666, -38.40000000000000568, 4.312909747525784709 ) ) ;
#7827 = CARTESIAN_POINT ( 'NONE',  ( 1.891708078845682595, -40.43301269999998482, -99.69999999890752918 ) ) ;
#7828 = DIRECTION ( 'NONE',  ( 0.000000000000000000, 0.000000000000000000, 1.000000000000000000 ) ) ;
#7829 = CARTESIAN_POINT ( 'NONE',  ( -4.566987299999997418, -46.89170807884566727, -96.99999999890751212 ) ) ;
#7830 = PRODUCT_RELATED_PRODUCT_CATEGORY ( 'part', '', ( #7049 ) ) ;
#7831 = SURFACE_SIDE_STYLE ('',( #4438 ) ) ;
#7832 = VERTEX_POINT ( 'NONE', #5997 ) ;
#7833 = CARTESIAN_POINT ( 'NONE',  ( -36.75497492228666374, -33.99859572486943904, -6.680053920257780220 ) ) ;
#7834 = CARTESIAN_POINT ( 'NONE',  ( -21.12512167993187973, -30.35140427513058015, 4.584493831696868860 ) ) ;
#7835 = ORIENTED_EDGE ( 'NONE', *, *, #793, .F. ) ;
#7836 = CARTESIAN_POINT ( 'NONE',  ( -20.62524821624488069, -33.20140427513057091, 1.538452329860250378 ) ) ;
#7837 = LINE ( 'NONE', #6996, #3354 ) ;
#7838 = CARTESIAN_POINT ( 'NONE',  ( -25.64110105645932336, -8.999999999999998224, 125.0000000000000000 ) ) ;
#7839 = CARTESIAN_POINT ( 'NONE',  ( 3.535533905932737309, -48.53553390593270933, -95.50000000000000000 ) ) ;
#7840 = DIRECTION ( 'NONE',  ( 0.000000000000000000, 0.5150380749100549327, 0.8571673007021118895 ) ) ;
#7841 = CARTESIAN_POINT ( 'NONE',  ( -4.999999999999998224, -42.92893218813448897, -95.04999999999999716 ) ) ;
#7842 = ORIENTED_EDGE ( 'NONE', *, *, #6341, .F. ) ;
#7843 = CARTESIAN_POINT ( 'NONE',  ( -23.98959235991431171, -40.50000000000000711, 6.010407640085604797 ) ) ;
#7844 = EDGE_CURVE ( 'NONE', #1476, #3394, #6610, .T. ) ;
#7845 = CIRCLE ( 'NONE', #5166, 1.649999999999998579 ) ;
#7846 = EDGE_LOOP ( 'NONE', ( #6377, #4654, #6684, #1583 ) ) ;
#7847 = CARTESIAN_POINT ( 'NONE',  ( -3.535533905932735532, -48.53553390593270933, -97.29999999999999716 ) ) ;
#7848 = STYLED_ITEM ( 'NONE', ( #2957 ), #85 ) ;
#7849 = CYLINDRICAL_SURFACE ( 'NONE', #4653, 1.649999999999998579 ) ;
#7850 = PLANE ( 'NONE',  #5426 ) ;
#7851 = DIRECTION ( 'NONE',  ( -0.000000000000000000, -0.000000000000000000, -1.000000000000000000 ) ) ;
#7852 = AXIS2_PLACEMENT_3D ( 'NONE', #1048, #7796, #339 ) ;
#7853 = APPLICATION_CONTEXT ( 'automotive_design' ) ;
#7854 = DIRECTION ( 'NONE',  ( -0.000000000000000000, 0.000000000000000000, -1.000000000000000000 ) ) ;
#7855 = CARTESIAN_POINT ( 'NONE',  ( -41.99999999999996447, 60.00000000000002842, -22.00000000000000000 ) ) ;
#7856 = DIRECTION ( 'NONE',  ( -0.000000000000000000, -0.000000000000000000, 1.000000000000000000 ) ) ;
#7857 = CARTESIAN_POINT ( 'NONE',  ( -38.46456197978948666, -47.40000000000001279, 4.312909747525784709 ) ) ;
#7858 = ADVANCED_FACE ( 'NONE', ( #4633 ), #6483, .F. ) ;
#7859 = DIRECTION ( 'NONE',  ( 0.000000000000000000, 1.000000000000000000, 0.000000000000000000 ) ) ;
#7860 = ORIENTED_EDGE ( 'NONE', *, *, #1, .F. ) ;
#7861 = CARTESIAN_POINT ( 'NONE',  ( -23.95213185889994989, -50.49859572486944614, 5.972947139071243861 ) ) ;
#7862 = CARTESIAN_POINT ( 'NONE',  ( -31.56260684030781505, -37.94999999999998153, 9.865911304835510265 ) ) ;
#7863 = CARTESIAN_POINT ( 'NONE',  ( -21.16389173201424612, -36.05140427513057944, -1.343104241417630185 ) ) ;
#7864 = VECTOR ( 'NONE', #2252, 1000.000000000000000 ) ;
#7865 = CARTESIAN_POINT ( 'NONE',  ( -3.535533905932736864, -41.46446609406723383, -95.90000000000000568 ) ) ;
#7866 = CARTESIAN_POINT ( 'NONE',  ( -30.00000000000002842, 0.000000000000000000, -29.65000000000000213 ) ) ;
#7867 = CARTESIAN_POINT ( 'NONE',  ( -21.07454398712378918, -35.34859572486944046, 4.485229520447505003 ) ) ;
#7868 = CARTESIAN_POINT ( 'NONE',  ( -21.53543802021056663, -36.90000000000000568, -4.312909747525783821 ) ) ;
#7869 = FACE_OUTER_BOUND ( 'NONE', #6812, .T. ) ;
#7870 = CARTESIAN_POINT ( 'NONE',  ( 50.00000000000002842, -44.99999999999997158, -2.099999999999997868 ) ) ;
#7871 = CARTESIAN_POINT ( 'NONE',  ( 4.566987299999998307, -44.99999999999997158, -99.84999999890752065 ) ) ;
#7872 =( NAMED_UNIT ( * ) SI_UNIT ( $, .STERADIAN. ) SOLID_ANGLE_UNIT ( ) );
#7873 = EDGE_LOOP ( 'NONE', ( #4864, #5018, #2366, #783 ) ) ;
#7874 = LINE ( 'NONE', #7165, #4550 ) ;
#7875 = CARTESIAN_POINT ( 'NONE',  ( -37.54950433343896776, -51.39859572486944472, 3.906122232810848249 ) ) ;
#7876 = CARTESIAN_POINT ( 'NONE',  ( -38.87487832006816291, -34.85140427513057659, -4.584493831696867971 ) ) ;
#7877 = EDGE_LOOP ( 'NONE', ( #2604, #1894, #6030, #851 ) ) ;
#7878 = VERTEX_POINT ( 'NONE', #8563 ) ;
#7879 = CARTESIAN_POINT ( 'NONE',  ( -38.87487832006816291, -31.85140427513056594, -4.584493831696867971 ) ) ;
#7880 = EDGE_CURVE ( 'NONE', #8429, #4408, #4268, .T. ) ;
#7881 = CARTESIAN_POINT ( 'NONE',  ( 34.99999999999998579, -44.99999999999995737, 30.00000000000000000 ) ) ;
#7882 = CARTESIAN_POINT ( 'NONE',  ( -30.00000000000002842, -57.51075773784449296, 0.000000000000000000 ) ) ;
#7883 = CARTESIAN_POINT ( 'NONE',  ( 5.000000000000003553, -42.92893218813449607, -97.64999999781502993 ) ) ;
#7884 = DIRECTION ( 'NONE',  ( 0.000000000000000000, 0.000000000000000000, 1.000000000000000000 ) ) ;
#7885 = CARTESIAN_POINT ( 'NONE',  ( 5.000000000000000000, -47.07106781186545419, -97.04999999999999716 ) ) ;
#7886 = ORIENTED_EDGE ( 'NONE', *, *, #8086, .T. ) ;
#7887 = CARTESIAN_POINT ( 'NONE',  ( -37.96330746473829976, -44.85000000000001563, -4.057507815433013754 ) ) ;
#7888 = AXIS2_PLACEMENT_3D ( 'NONE', #3901, #1957, #2625 ) ;
#7889 = ORIENTED_EDGE ( 'NONE', *, *, #7070, .F. ) ;
#7890 = CARTESIAN_POINT ( 'NONE',  ( 4.999999999999998224, -44.99999999999997158, -98.60000000000000853 ) ) ;
#7891 = CARTESIAN_POINT ( 'NONE',  ( -50.00000000000002842, 30.00000000000000000, 60.00000000000002842 ) ) ;
#7892 = CARTESIAN_POINT ( 'NONE',  ( -24.02705286092866643, -36.50140427513057517, 6.047868141099968398 ) ) ;
#7893 = ADVANCED_FACE ( 'NONE', ( #4904 ), #8079, .F. ) ;
#7894 = AXIS2_PLACEMENT_3D ( 'NONE', #1314, #5455, #1359 ) ;
#7895 = PLANE ( 'NONE',  #2515 ) ;
#7896 = CARTESIAN_POINT ( 'NONE',  ( -25.94249218456686279, -37.65000000000000568, 7.963307464738194952 ) ) ;
#7897 = DIRECTION ( 'NONE',  ( -0.000000000000000000, -0.000000000000000000, -1.000000000000000000 ) ) ;
#7898 = CARTESIAN_POINT ( 'NONE',  ( -36.71751442127229836, -48.00000000000000711, -6.717514421272142044 ) ) ;
#7899 = EDGE_CURVE ( 'NONE', #344, #8009, #704, .T. ) ;
#7900 = CARTESIAN_POINT ( 'NONE',  ( 42.00000000000000711, 84.00000000000002842, 21.99999999999992184 ) ) ;
#7901 = ORIENTED_EDGE ( 'NONE', *, *, #7524, .F. ) ;
#7902 = CARTESIAN_POINT ( 'NONE',  ( -34.10713997105786888, -46.14859572486944472, -7.938018618334151455 ) ) ;
#7903 = CARTESIAN_POINT ( 'NONE',  ( -38.46456197978948666, -38.40000000000000568, 4.312909747525784709 ) ) ;
#7904 = CARTESIAN_POINT ( 'NONE',  ( -31.27736804086391942, -41.30140427513058654, -8.403638346957361449 ) ) ;
#7905 = MECHANICAL_DESIGN_GEOMETRIC_PRESENTATION_REPRESENTATION (  '', ( #722 ), #1432 ) ;
#7906 = FACE_BOUND ( 'NONE', #959, .T. ) ;
#7907 = DIRECTION ( 'NONE',  ( -1.000000000000000000, 0.000000000000000000, 0.000000000000000000 ) ) ;
#7908 = CARTESIAN_POINT ( 'NONE',  ( -25.41550616830297571, -38.64859572486943762, 8.874878320068054549 ) ) ;
#7909 = CARTESIAN_POINT ( 'NONE',  ( -25.46513832392765408, -40.65000000000000568, 8.900167166472096270 ) ) ;
#7910 = AXIS2_PLACEMENT_3D ( 'NONE', #4576, #1968, #8105 ) ;
#7911 = CARTESIAN_POINT ( 'NONE',  ( 0.000000000000000000, 0.000000000000000000, 0.000000000000000000 ) ) ;
#7912 = CARTESIAN_POINT ( 'NONE',  ( -50.00000000000002842, 30.00000000000000000, 60.00000000000002842 ) ) ;
#7913 = CARTESIAN_POINT ( 'NONE',  ( -4.566987299999998307, -44.99999999999997158, -99.44999999890752918 ) ) ;
#7914 = AXIS2_PLACEMENT_3D ( 'NONE', #5635, #7664, #2300 ) ;
#7915 = VERTEX_POINT ( 'NONE', #4109 ) ;
#7916 = FACE_OUTER_BOUND ( 'NONE', #7564, .T. ) ;
#7917 = EDGE_CURVE ( 'NONE', #1009, #5895, #5372, .T. ) ;
#7918 = CARTESIAN_POINT ( 'NONE',  ( -33.81171626276147890, -51.09859572486944046, 7.597606577763319713 ) ) ;
#7919 = CARTESIAN_POINT ( 'NONE',  ( -34.36011273255026310, -31.10140427513058370, 8.440510857627391061 ) ) ;
#7920 = ORIENTED_EDGE ( 'NONE', *, *, #4106, .F. ) ;
#7921 = AXIS2_PLACEMENT_3D ( 'NONE', #5188, #461, #5150 ) ;
#7922 = CARTESIAN_POINT ( 'NONE',  ( -38.87487832006816291, -37.85140427513057659, -4.584493831696867971 ) ) ;
#7923 = CARTESIAN_POINT ( 'NONE',  ( -50.00000000000002842, -44.99999999999997158, 2.099999999999997868 ) ) ;
#7924 = CARTESIAN_POINT ( 'NONE',  ( -2.071067811865475061, -39.99999999999997158, -99.14999999999999147 ) ) ;
#7925 = DIRECTION ( 'NONE',  ( 0.000000000000000000, 0.000000000000000000, 1.000000000000000000 ) ) ;
#7926 = CARTESIAN_POINT ( 'NONE',  ( 45.00000000000003553, -44.99999999999997158, 0.000000000000000000 ) ) ;
#7927 = EDGE_LOOP ( 'NONE', ( #7467, #7774, #6863, #3991 ) ) ;
#7928 = CARTESIAN_POINT ( 'NONE',  ( -26.14108075221394856, -39.60000000000000853, -7.573555455601170827 ) ) ;
#7929 = EDGE_LOOP ( 'NONE', ( #8470, #2187 ) ) ;
#7930 = CARTESIAN_POINT ( 'NONE',  ( 34.00000000000000000, 0.000000000000000000, 1.610000000000000098 ) ) ;
#7931 = CARTESIAN_POINT ( 'NONE',  ( -3.535533905932735532, -48.53553390593270933, -96.50000000000000000 ) ) ;
#7932 = CARTESIAN_POINT ( 'NONE',  ( -22.93678734525658314, -45.74999999999999289, -7.063212654743582952 ) ) ;
#7933 = CARTESIAN_POINT ( 'NONE',  ( -4.566987299999998307, -43.10829192115428299, -97.69999999890751496 ) ) ;
#7934 = CARTESIAN_POINT ( 'NONE',  ( 4.966556519403932946, -45.64283254358549158, -99.99918711676903627 ) ) ;
#7935 = CARTESIAN_POINT ( 'NONE',  ( -36.35910488754074521, -37.25140427513058228, 6.280328284105565650 ) ) ;
#7936 = AXIS2_PLACEMENT_3D ( 'NONE', #3690, #6413, #7081 ) ;
#7937 = ADVANCED_FACE ( 'NONE', ( #6700 ), #4195, .T. ) ;
#7938 = CARTESIAN_POINT ( 'NONE',  ( 3.535533905932737309, -48.53553390593270933, -96.99999999781503845 ) ) ;
#7939 =( BOUNDED_CURVE ( )  B_SPLINE_CURVE ( 2, ( #5722, #7130, #7839, #8424, #3788, #7753, #4404, #4487, #1093 ),
 .UNSPECIFIED., .F., .T. ) 
 B_SPLINE_CURVE_WITH_KNOTS ( ( 3, 2, 2, 2, 3 ),
 ( 0.07142857142857145236, 0.08928571428571430157, 0.1071428571428571369, 0.1249999999999999861, 0.1428571428571428215 ),
 .UNSPECIFIED. ) 
 CURVE ( )  GEOMETRIC_REPRESENTATION_ITEM ( )  RATIONAL_B_SPLINE_CURVE ( ( 0.9999999999999998890, 0.9238795325112868495, 1.000000000000000000, 0.9238795325112867385, 1.000000000000000000, 0.9238795325112867385, 1.000000000000000000, 0.9238795325112868495, 0.9999999999999998890 ) ) 
 REPRESENTATION_ITEM ( '' )  );
#7940 = CARTESIAN_POINT ( 'NONE',  ( -37.57355545560112375, -32.40000000000000568, 3.858919247786223305 ) ) ;
#7941 = EDGE_CURVE ( 'NONE', #8141, #5715, #52, .T. ) ;
#7942 = CARTESIAN_POINT ( 'NONE',  ( 4.999999999999998224, -44.99999999999997158, -97.79999999999999716 ) ) ;
#7943 = CARTESIAN_POINT ( 'NONE',  ( -34.31290974752564438, -47.10000000000000142, 8.464561979789547053 ) ) ;
#7944 = VERTEX_POINT ( 'NONE', #5461 ) ;
#7945 = CARTESIAN_POINT ( 'NONE',  ( -38.81868038277247734, -51.54859572486944330, 1.453139578080855365 ) ) ;
#7946 = CARTESIAN_POINT ( 'NONE',  ( -25.68709025247441602, -39.60000000000000853, -8.464561979789547053 ) ) ;
#7947 = CARTESIAN_POINT ( 'NONE',  ( -24.02705286092866643, -42.50140427513057517, 6.047868141099968398 ) ) ;
#7948 = EDGE_CURVE ( 'NONE', #8538, #1354, #8218, .T. ) ;
#7949 = CARTESIAN_POINT ( 'NONE',  ( 0.000000000000000000, 1.773042676681340968, -1.951563910473907981E-15 ) ) ;
#7950 = CARTESIAN_POINT ( 'NONE',  ( -45.00000000000003553, -44.99999999999997158, -2.099999999999997868 ) ) ;
#7951 = CARTESIAN_POINT ( 'NONE',  ( -34.26570676250101855, -36.09859572486943335, 8.488613101951703044 ) ) ;
#7952 = CARTESIAN_POINT ( 'NONE',  ( -38.90016716647221529, -41.84999999999999432, -4.534861676072185155 ) ) ;
#7953 = DIRECTION ( 'NONE',  ( -1.000000000000000000, -0.000000000000000000, -0.000000000000000000 ) ) ;
#7954 = DIRECTION ( 'NONE',  ( 1.000000000000000000, -0.000000000000000000, -0.000000000000000000 ) ) ;
#7955 = CARTESIAN_POINT ( 'NONE',  ( -4.566987299999997418, -46.89170807884566727, -98.59999999890753486 ) ) ;
#7956 = SURFACE_STYLE_USAGE ( .BOTH. , #3295 ) ;
#7957 = ORIENTED_EDGE ( 'NONE', *, *, #4150, .F. ) ;
#7958 = FACE_BOUND ( 'NONE', #897, .T. ) ;
#7959 = CARTESIAN_POINT ( 'NONE',  ( -36.28032828410546529, -48.24859572486943904, 6.359104887540839357 ) ) ;
#7960 = CARTESIAN_POINT ( 'NONE',  ( -34.48522952044771017, -32.15140427513058086, -8.925456012876139766 ) ) ;
#7961 = EDGE_CURVE ( 'NONE', #196, #5319, #5910, .T. ) ;
#7962 = ORIENTED_EDGE ( 'NONE', *, *, #2371, .T. ) ;
#7963 = ORIENTED_EDGE ( 'NONE', *, *, #1148, .F. ) ;
#7964 = CARTESIAN_POINT ( 'NONE',  ( -20.62524821624488069, -45.20140427513059223, 1.538452329860250378 ) ) ;
#7965 = ADVANCED_FACE ( 'NONE', ( #797 ), #2132, .F. ) ;
#7966 = DIRECTION ( 'NONE',  ( 0.000000000000000000, 0.000000000000000000, -1.000000000000000000 ) ) ;
#7967 = CARTESIAN_POINT ( 'NONE',  ( -18.00000000000002132, 1.469576158976823947E-15, -28.65000000000000213 ) ) ;
#7968 = CARTESIAN_POINT ( 'NONE',  ( -3.535533905932736864, -41.46446609406723383, -99.79999999781504982 ) ) ;
#7969 = CARTESIAN_POINT ( 'NONE',  ( 30.33389005480432132, -49.99999999999995026, 12.49999999999997158 ) ) ;
#7970 = CARTESIAN_POINT ( 'NONE',  ( 4.999999999999998224, -42.92893218813448897, -99.35000000000000853 ) ) ;
#7971 = VERTEX_POINT ( 'NONE', #6831 ) ;
#7972 =( REPRESENTATION_RELATIONSHIP ('NONE','NONE', #2265, #7373 ) REPRESENTATION_RELATIONSHIP_WITH_TRANSFORMATION ( #8304 )SHAPE_REPRESENTATION_RELATIONSHIP( ) );
#7973 = EDGE_CURVE ( 'NONE', #2290, #1795, #6177, .T. ) ;
#7974 = CARTESIAN_POINT ( 'NONE',  ( -36.31971658582311591, -38.25000000000001421, 6.319716585823199395 ) ) ;
#7975 = VECTOR ( 'NONE', #5000, 1000.000000000000000 ) ;
#7976 = EDGE_LOOP ( 'NONE', ( #3205, #2705, #3136, #1342 ) ) ;
#7977 = CARTESIAN_POINT ( 'NONE',  ( -4.783493649999997821, -44.99999999999997158, -95.12499999945376317 ) ) ;
#7978 = CARTESIAN_POINT ( 'NONE',  ( 4.999999999999998224, -44.99999999999997158, -96.89999999781505835 ) ) ;
#7979 = CARTESIAN_POINT ( 'NONE',  ( -34.53486167607238144, -45.14999999999999858, -8.900167166472096270 ) ) ;
#7980 = CARTESIAN_POINT ( 'NONE',  ( -1.891708078845683039, -40.43301269999998482, -98.59999999890754907 ) ) ;
#7981 = AXIS2_PLACEMENT_3D ( 'NONE', #1395, #731, #6162 ) ;
#7982 = CARTESIAN_POINT ( 'NONE',  ( 5.004075312705366763, -44.80061875307438157, -100.0004355954672093 ) ) ;
#7983 = CARTESIAN_POINT ( 'NONE',  ( -37.59760657776328685, -31.40140427513058086, 3.811716262761598362 ) ) ;
#7984 = AXIS2_PLACEMENT_3D ( 'NONE', #4030, #6006, #8039 ) ;
#7985 = EDGE_CURVE ( 'NONE', #5875, #4613, #6525, .T. ) ;
#7986 = CARTESIAN_POINT ( 'NONE',  ( -3.535533905932736864, -41.46446609406723383, -97.49300000002185129 ) ) ;
#7987 = CARTESIAN_POINT ( 'NONE',  ( -31.32969295284206979, -33.30000000000000426, -8.395350895058669494 ) ) ;
#7988 = CARTESIAN_POINT ( 'NONE',  ( -35.35889894354067309, -7.999999999999996447, -24.00000000000000000 ) ) ;
#7989 = CARTESIAN_POINT ( 'NONE',  ( -38.90016716647221529, -47.85000000000000142, -4.534861676072185155 ) ) ;
#7990 = AXIS2_PLACEMENT_3D ( 'NONE', #6526, #3066, #6481 ) ;
#7991 = DIRECTION ( 'NONE',  ( 6.123233995736766036E-17, -1.000000000000000000, 0.000000000000000000 ) ) ;
#7992 = ORIENTED_EDGE ( 'NONE', *, *, #2313, .F. ) ;
#7993 = DIRECTION ( 'NONE',  ( -0.000000000000000000, 0.000000000000000000, 1.000000000000000000 ) ) ;
#7994 = CARTESIAN_POINT ( 'NONE',  ( -39.86591130483550671, -41.55000000000001137, 1.562606840307984468 ) ) ;
#7995 = CARTESIAN_POINT ( 'NONE',  ( -33.85891924778610473, -32.10000000000000142, 7.573555455601171715 ) ) ;
#7996 =( BOUNDED_CURVE ( )  B_SPLINE_CURVE ( 2, ( #7540, #269, #800, #5556, #5646, #8262, #1502, #2312, #4197, #7500, #7674, #1639, #2224, #4331, #7011 ),
 .UNSPECIFIED., .F., .T. ) 
 B_SPLINE_CURVE_WITH_KNOTS ( ( 3, 2, 2, 2, 2, 2, 2, 3 ),
 ( 0.7678571432794624174, 0.7857142857142856984, 0.8035714285714286031, 0.8214285714285713969, 0.8392857142857143016, 0.8571428571428570953, 0.8750000000000000000, 0.8928571428571429047 ),
 .UNSPECIFIED. ) 
 CURVE ( )  GEOMETRIC_REPRESENTATION_ITEM ( )  RATIONAL_B_SPLINE_CURVE ( ( 1.000000000000000000, 0.9238795325112867385, 1.000000000000000000, 0.9238795325112867385, 1.000000000000000000, 0.9238795325112867385, 1.000000000000000000, 0.9238795325112867385, 1.000000000000000000, 0.9238795325112867385, 1.000000000000000000, 0.9238795325112867385, 1.000000000000000000, 0.9238795325112867385, 1.000000000000000000 ) ) 
 REPRESENTATION_ITEM ( '' )  );
#7997 = DIRECTION ( 'NONE',  ( -0.000000000000000000, -0.000000000000000000, 1.000000000000000000 ) ) ;
#7998 = DIRECTION ( 'NONE',  ( 1.000000000000000000, -0.000000000000000000, -0.000000000000000000 ) ) ;
#7999 = CARTESIAN_POINT ( 'NONE',  ( -34.58449383169706692, -37.14859572486943762, -8.874878320068054549 ) ) ;
#8000 = CARTESIAN_POINT ( 'NONE',  ( 42.00000000000000711, -21.99999999999992184, 80.00000000000002842 ) ) ;
#8001 = DIRECTION ( 'NONE',  ( 0.000000000000000000, 1.000000000000000000, 0.000000000000000000 ) ) ;
#8002 = CARTESIAN_POINT ( 'NONE',  ( -4.566987299999997418, -46.89170807884566727, -100.1999999989075150 ) ) ;
#8003 = ORIENTED_EDGE ( 'NONE', *, *, #6513, .F. ) ;
#8004 = CARTESIAN_POINT ( 'NONE',  ( -4.999999999999998224, -44.99999999999997158, -99.00000000000000000 ) ) ;
#8005 = CARTESIAN_POINT ( 'NONE',  ( -38.82739432537914581, -47.54999999999999716, 1.398121909749243441 ) ) ;
#8006 = CARTESIAN_POINT ( 'NONE',  ( -25.73429323749904185, -31.59859572486943335, -8.488613101951701267 ) ) ;
#8007 = CARTESIAN_POINT ( 'NONE',  ( -31.43380250590416125, -29.30140427513058299, -9.391326687552492558 ) ) ;
#8008 = ADVANCED_FACE ( 'NONE', ( #7538 ), #7662, .F. ) ;
#8009 = VERTEX_POINT ( 'NONE', #750 ) ;
#8010 = ORIENTED_EDGE ( 'NONE', *, *, #723, .F. ) ;
#8011 = CARTESIAN_POINT ( 'NONE',  ( -21.51138689804841420, -47.90140427513058086, -4.265706762501151772 ) ) ;
#8012 = CYLINDRICAL_SURFACE ( 'NONE', #6779, 9.999999999999994671 ) ;
#8013 = CARTESIAN_POINT ( 'NONE',  ( -2.071067811865475061, -39.99999999999997158, -98.24999999781506688 ) ) ;
#8014 = CARTESIAN_POINT ( 'NONE',  ( -4.999999999999998224, -42.92893218813449607, -95.04999999999999716 ) ) ;
#8015 = CARTESIAN_POINT ( 'NONE',  ( -3.535533905932735532, -48.53553390593270933, -98.90000000000000568 ) ) ;
#8016 = ORIENTED_EDGE ( 'NONE', *, *, #7645, .F. ) ;
#8017 = CARTESIAN_POINT ( 'NONE',  ( -21.17260567462091458, -46.05000000000001137, -1.398121909749242331 ) ) ;
#8018 = DIRECTION ( 'NONE',  ( -0.000000000000000000, -0.000000000000000000, 1.000000000000000000 ) ) ;
#8019 = EDGE_LOOP ( 'NONE', ( #6373, #2804, #1994, #2433 ) ) ;
#8020 = CARTESIAN_POINT ( 'NONE',  ( 3.229347689422841228, -48.22934768942280925, -97.54999999890752349 ) ) ;
#8021 = CARTESIAN_POINT ( 'NONE',  ( 3.535533905932736420, -41.46446609406723383, -95.99999999781503845 ) ) ;
#8022 = CARTESIAN_POINT ( 'NONE',  ( -23.28248557872775137, -46.50000000000000711, 6.717514421272141156 ) ) ;
#8023 = CARTESIAN_POINT ( 'NONE',  ( 3.229347689422841228, -48.22934768942280925, -98.14999999890753202 ) ) ;
#8024 =( REPRESENTATION_RELATIONSHIP ('NONE','NONE', #2265, #4396 ) REPRESENTATION_RELATIONSHIP_WITH_TRANSFORMATION ( #705 )SHAPE_REPRESENTATION_RELATIONSHIP( ) );
#8025 = DIRECTION ( 'NONE',  ( -1.000000000000000000, 0.000000000000000000, 0.000000000000000000 ) ) ;
#8026 = CARTESIAN_POINT ( 'NONE',  ( -31.45313957808072303, -33.95140427513058512, 8.818680382772479120 ) ) ;
#8027 = CARTESIAN_POINT ( 'NONE',  ( -3.061616997868382155E-16, -39.99999999999997158, -96.79300000002184845 ) ) ;
#8028 = UNCERTAINTY_MEASURE_WITH_UNIT (LENGTH_MEASURE( 1.000000000000000082E-05 ), #490, 'distance_accuracy_value', 'NONE');
#8029 = VECTOR ( 'NONE', #7547, 1000.000000000000114 ) ;
#8030 = CARTESIAN_POINT ( 'NONE',  ( -37.96330746473829976, -38.85000000000000853, -4.057507815433013754 ) ) ;
#8031 = CARTESIAN_POINT ( 'NONE',  ( -3.535533905932736864, -41.46446609406723383, -97.50000000000000000 ) ) ;
#8032 = DIRECTION ( 'NONE',  ( -0.000000000000000000, -1.000000000000000000, -0.000000000000000000 ) ) ;
#8033 = AXIS2_PLACEMENT_3D ( 'NONE', #1017, #7583, #7057 ) ;
#8034 = ORIENTED_EDGE ( 'NONE', *, *, #5114, .T. ) ;
#8035 = LINE ( 'NONE', #5, #4050 ) ;
#8036 = CARTESIAN_POINT ( 'NONE',  ( -34.31290974752564438, -44.10000000000000853, 8.464561979789547053 ) ) ;
#8037 = CARTESIAN_POINT ( 'NONE',  ( -34.05750781543318340, -30.15000000000000213, -7.963307464738195840 ) ) ;
#8038 = DIRECTION ( 'NONE',  ( 0.000000000000000000, 0.000000000000000000, 1.000000000000000000 ) ) ;
#8039 = DIRECTION ( 'NONE',  ( 0.000000000000000000, 0.000000000000000000, 1.000000000000000000 ) ) ;
#8040 = CARTESIAN_POINT ( 'NONE',  ( -31.53845232986046554, -34.29859572486943620, -9.374751783755117529 ) ) ;
#8041 = FACE_OUTER_BOUND ( 'NONE', #550, .T. ) ;
#8042 = FACE_OUTER_BOUND ( 'NONE', #8019, .T. ) ;
#8043 = CARTESIAN_POINT ( 'NONE',  ( -3.229347689422839451, -48.22934768942280925, -95.94999999890752918 ) ) ;
#8044 =( LENGTH_UNIT ( ) NAMED_UNIT ( * ) SI_UNIT ( .MILLI., .METRE. ) );
#8045 = ORIENTED_EDGE ( 'NONE', *, *, #6388, .F. ) ;
#8046 = CARTESIAN_POINT ( 'NONE',  ( 50.00000000000002842, -59.99999999999997158, 30.00000000000000000 ) ) ;
#8047 = CARTESIAN_POINT ( 'NONE',  ( -22.03669253526174998, -49.35000000000000853, 4.057507815433014642 ) ) ;
#8048 = CARTESIAN_POINT ( 'NONE',  ( -20.60867331244750034, -35.19859572486944188, 1.433802505903951419 ) ) ;
#8049 = CARTESIAN_POINT ( 'NONE',  ( -22.89739904353894318, -41.75140427513057517, -7.023824353025938549 ) ) ;
#8050 = EDGE_LOOP ( 'NONE', ( #7085, #65, #5431 ) ) ;
#8051 = ORIENTED_EDGE ( 'NONE', *, *, #7702, .F. ) ;
#8052 = CARTESIAN_POINT ( 'NONE',  ( -25.51477047955235378, -42.65140427513058086, 8.925456012876139766 ) ) ;
#8053 = DIRECTION ( 'NONE',  ( 0.000000000000000000, 0.000000000000000000, 1.000000000000000000 ) ) ;
#8054 = DIRECTION ( 'NONE',  ( 0.000000000000000000, -8.560894001270036306E-16, -1.000000000000000000 ) ) ;
#8055 = CARTESIAN_POINT ( 'NONE',  ( -4.999999999999998224, -42.92893218813448897, -99.74999999781503845 ) ) ;
#8056 = CARTESIAN_POINT ( 'NONE',  ( -41.99999999999996447, -22.00000000000000000, 80.00000000000002842 ) ) ;
#8057 = DIRECTION ( 'NONE',  ( 0.000000000000000000, 1.000000000000000000, 0.000000000000000000 ) ) ;
#8058 = VERTEX_POINT ( 'NONE', #1412 ) ;
#8059 = CARTESIAN_POINT ( 'NONE',  ( -28.61798213517984024, -32.79859572486943620, 8.387063443159973986 ) ) ;
#8060 = ADVANCED_FACE ( 'NONE', ( #6220 ), #4153, .T. ) ;
#8061 = CARTESIAN_POINT ( 'NONE',  ( -20.61696076434619584, -37.20000000000000284, 1.486127417882100676 ) ) ;
#8062 = AXIS2_PLACEMENT_3D ( 'NONE', #7764, #1732, #4418 ) ;
#8063 = ORIENTED_EDGE ( 'NONE', *, *, #735, .F. ) ;
#8064 = CARTESIAN_POINT ( 'NONE',  ( 8.389419568037416259E-16, -49.56698729999997255, -97.64999999890751781 ) ) ;
#8065 = EDGE_CURVE ( 'NONE', #5982, #8403, #4814, .T. ) ;
#8066 = CARTESIAN_POINT ( 'NONE',  ( 9.184850993605145972E-16, -49.99999999999997158, -97.09999999781504698 ) ) ;
#8067 = CARTESIAN_POINT ( 'NONE',  ( -37.06321265474346660, -41.25000000000000711, 7.063212654743582952 ) ) ;
#8068 = CARTESIAN_POINT ( 'NONE',  ( 1.891708078845685481, -49.56698729999997255, -98.19999999890751496 ) ) ;
#8069 = VECTOR ( 'NONE', #839, 1000.000000000000000 ) ;
#8070 = FACE_OUTER_BOUND ( 'NONE', #297, .T. ) ;
#8071 = COLOUR_RGB ( '', 0.31764706, 0.68627451, 0.89019608) ;
#8072 = CARTESIAN_POINT ( 'NONE',  ( -28.54686042191934092, -29.45140427513057801, -8.818680382772479120 ) ) ;
#8073 = ADVANCED_FACE ( 'NONE', ( #4862 ), #5554, .T. ) ;
#8074 = VECTOR ( 'NONE', #906, 1000.000000000000000 ) ;
#8075 = CARTESIAN_POINT ( 'NONE',  ( 2.071067811865477282, -49.99999999999996447, -97.14300000002185698 ) ) ;
#8076 = CARTESIAN_POINT ( 'NONE',  ( -33.85891924778610473, -38.10000000000000853, 7.573555455601171715 ) ) ;
#8077 = EDGE_CURVE ( 'NONE', #7944, #7472, #4372, .T. ) ;
#8078 = CARTESIAN_POINT ( 'NONE',  ( 3.535533905932736420, -41.46446609406723383, -97.69999999999998863 ) ) ;
#8079 = CYLINDRICAL_SURFACE ( 'NONE', #3839, 1.000000000000000888 ) ;
#8080 = AXIS2_PLACEMENT_3D ( 'NONE', #5887, #2497, #8660 ) ;
#8081 = APPLICATION_PROTOCOL_DEFINITION ( 'draft international standard', 'automotive_design', 1998, #6951 ) ;
#8082 = ORIENTED_EDGE ( 'NONE', *, *, #4137, .T. ) ;
#8083 = DIRECTION ( 'NONE',  ( 0.000000000000000000, 0.000000000000000000, -1.000000000000000000 ) ) ;
#8084 = CARTESIAN_POINT ( 'NONE',  ( -25.68709025247441602, -42.60000000000000853, -8.464561979789547053 ) ) ;
#8085 = CARTESIAN_POINT ( 'NONE',  ( -21.16389173201424612, -45.05140427513057944, -1.343104241417630185 ) ) ;
#8086 = EDGE_CURVE ( 'NONE', #3680, #7609, #2307, .T. ) ;
#8087 = AXIS2_PLACEMENT_3D ( 'NONE', #4205, #7466, #1555 ) ;
#8088 = DIRECTION ( 'NONE',  ( -1.000000000000000000, -0.000000000000000000, -0.000000000000000000 ) ) ;
#8089 = CARTESIAN_POINT ( 'NONE',  ( 34.55267497488053863, -42.92638634940914955, 11.64163759925509822 ) ) ;
#8090 = CARTESIAN_POINT ( 'NONE',  ( -21.07454398712378918, -47.34859572486942625, 4.485229520447505003 ) ) ;
#8091 = DIRECTION ( 'NONE',  ( 1.000000000000000000, 0.000000000000000000, 0.000000000000000000 ) ) ;
#8092 = CARTESIAN_POINT ( 'NONE',  ( -34.53486167607238855, -30.15000000000000568, -8.900167166472096270 ) ) ;
#8093 = CARTESIAN_POINT ( 'NONE',  ( -3.229347689422839451, -48.22934768942280925, -96.74999999890752633 ) ) ;
#8094 = SHAPE_REPRESENTATION_RELATIONSHIP ( 'NONE' , 'NONE' ,  #4062, #2772 ) ;
#8095 = ORIENTED_EDGE ( 'NONE', *, *, #6769, .F. ) ;
#8096 = DIRECTION ( 'NONE',  ( 1.000000000000000000, 0.000000000000000000, 0.000000000000000000 ) ) ;
#8097 = CARTESIAN_POINT ( 'NONE',  ( -28.60187809025093841, -45.45000000000000995, -8.827394325379140483 ) ) ;
#8098 = CARTESIAN_POINT ( 'NONE',  ( -34.26570676250101855, -36.09859572486943335, 8.488613101951703044 ) ) ;
#8099 = CARTESIAN_POINT ( 'NONE',  ( -38.48861310195163554, -43.40140427513058796, 4.265706762501153548 ) ) ;
#8100 = EDGE_CURVE ( 'NONE', #1663, #5109, #3569, .T. ) ;
#8101 = ORIENTED_EDGE ( 'NONE', *, *, #8303, .F. ) ;
#8102 = ORIENTED_EDGE ( 'NONE', *, *, #2327, .T. ) ;
#8103 = CARTESIAN_POINT ( 'NONE',  ( -39.37475178375516549, -49.70140427513058512, -1.538452329860249712 ) ) ;
#8104 = EDGE_CURVE ( 'NONE', #6156, #2506, #5921, .T. ) ;
#8105 = DIRECTION ( 'NONE',  ( -0.7071067811865587860, 0.000000000000000000, -0.7071067811865362485 ) ) ;
#8106 = CARTESIAN_POINT ( 'NONE',  ( -3.535533905932735532, -48.53553390593270933, -99.59999999781504698 ) ) ;
#8107 = LINE ( 'NONE', #1932, #3283 ) ;
#8108 = DIRECTION ( 'NONE',  ( 1.000000000000000000, 0.000000000000000000, -0.000000000000000000 ) ) ;
#8109 = ORIENTED_EDGE ( 'NONE', *, *, #4546, .F. ) ;
#8110 = CARTESIAN_POINT ( 'NONE',  ( -21.18131961722757595, -35.04859572486943620, -1.453139578080854699 ) ) ;
#8111 = CARTESIAN_POINT ( 'NONE',  ( -37.06321265474346660, -38.25000000000001421, 7.063212654743582952 ) ) ;
#8112 = AXIS2_PLACEMENT_3D ( 'NONE', #8437, #5649, #6399 ) ;
#8113 = VERTEX_POINT ( 'NONE', #4239 ) ;
#8114 = ORIENTED_EDGE ( 'NONE', *, *, #99, .F. ) ;
#8115 = CARTESIAN_POINT ( 'NONE',  ( 1.891708078845682595, -40.43301269999998482, -98.09999999890752065 ) ) ;
#8116 = CARTESIAN_POINT ( 'NONE',  ( 3.535533905932736420, -41.46446609406723383, -96.79999999781504982 ) ) ;
#8117 = CARTESIAN_POINT ( 'NONE',  ( -21.09983283352784156, -43.35000000000000853, 4.534861676072186043 ) ) ;
#8118 = CARTESIAN_POINT ( 'NONE',  ( 3.229347689422841228, -48.22934768942280925, -98.94999999890752918 ) ) ;
#8119 = DIRECTION ( 'NONE',  ( -1.000000000000000000, 0.000000000000000000, 0.000000000000000000 ) ) ;
#8120 = AXIS2_PLACEMENT_3D ( 'NONE', #7303, #6593, #1892 ) ;
#8121 = CARTESIAN_POINT ( 'NONE',  ( -31.45313957808072303, -42.95140427513058512, 8.818680382772479120 ) ) ;
#8122 = AXIS2_PLACEMENT_3D ( 'NONE', #4823, #846, #712 ) ;
#8123 = CARTESIAN_POINT ( 'NONE',  ( -3.535533905932736864, -41.46446609406723383, -95.89300000002184277 ) ) ;
#8124 = CARTESIAN_POINT ( 'NONE',  ( -26.14108075221394856, -45.60000000000000853, -7.573555455601170827 ) ) ;
#8125 = CARTESIAN_POINT ( 'NONE',  ( 28.69346486511991046, -49.83744928702510180, 12.43572992548470246 ) ) ;
#8126 = DIRECTION ( 'NONE',  ( 1.000000000000000000, 0.000000000000000000, 0.000000000000000000 ) ) ;
#8127 = APPLICATION_PROTOCOL_DEFINITION ( 'draft international standard', 'automotive_design', 1998, #7684 ) ;
#8128 = ORIENTED_EDGE ( 'NONE', *, *, #7144, .F. ) ;
#8129 = CARTESIAN_POINT ( 'NONE',  ( 2.000000000000000000, 1.773042676681340968, -1.951563910473907981E-15 ) ) ;
#8130 = VECTOR ( 'NONE', #1284, 1000.000000000000000 ) ;
#8131 = CARTESIAN_POINT ( 'NONE',  ( -21.53543802021056663, -45.90000000000001279, -4.312909747525783821 ) ) ;
#8132 = CARTESIAN_POINT ( 'NONE',  ( -37.57355545560112375, -32.40000000000000568, 3.858919247786223305 ) ) ;
#8133 = CIRCLE ( 'NONE', #653, 1.000000000000000888 ) ;
#8134 = CARTESIAN_POINT ( 'NONE',  ( -25.03350713684106665, -44.33520523457838891, 11.47122145076293798 ) ) ;
#8135 = TOROIDAL_SURFACE ( 'NONE', #509, 11.32499999999999929, 1.324999999999999956 ) ;
#8136 = DIRECTION ( 'NONE',  ( 1.000000000000000000, -0.000000000000000000, -0.000000000000000000 ) ) ;
#8137 = CARTESIAN_POINT ( 'NONE',  ( -22.97617564697422665, -46.74859572486943904, -7.102600956461224690 ) ) ;
#8138 = EDGE_CURVE ( 'NONE', #3221, #2177, #224, .T. ) ;
#8139 = DIRECTION ( 'NONE',  ( 1.000000000000000000, 0.000000000000000000, -0.000000000000000000 ) ) ;
#8140 = CARTESIAN_POINT ( 'NONE',  ( -3.535533905932735532, -48.53553390593270933, -99.59999999781504698 ) ) ;
#8141 = VERTEX_POINT ( 'NONE', #931 ) ;
#8142 = CARTESIAN_POINT ( 'NONE',  ( -33.35889894354067309, 8.000000000000000000, -23.99999999999999289 ) ) ;
#8143 = CARTESIAN_POINT ( 'NONE',  ( -37.98859631114233792, -33.84859572486942625, -4.007875659808334490 ) ) ;
#8144 = CARTESIAN_POINT ( 'NONE',  ( -25.41550616830297571, -38.64859572486943762, 8.874878320068054549 ) ) ;
#8145 = CARTESIAN_POINT ( 'NONE',  ( -28.56619749409589204, -42.80140427513057944, 9.391326687552490782 ) ) ;
#8146 = EDGE_LOOP ( 'NONE', ( #8003, #915, #5541, #3081, #2206, #2294 ) ) ;
#8147 = AXIS2_PLACEMENT_3D ( 'NONE', #1107, #6565, #6397 ) ;
#8148 = APPLICATION_CONTEXT ( 'automotive_design' ) ;
#8149 = VERTEX_POINT ( 'NONE', #3584 ) ;
#8150 = CARTESIAN_POINT ( 'NONE',  ( -39.87462524744216807, -46.55140427513058654, 1.507589171976367215 ) ) ;
#8151 = CARTESIAN_POINT ( 'NONE',  ( -7.654042494670954648E-16, -39.99999999999997158, -100.0000000000000000 ) ) ;
#8152 = CARTESIAN_POINT ( 'NONE',  ( -32.50890011656069589, -40.67193172067895546, 12.24650812517142207 ) ) ;
#8153 = CARTESIAN_POINT ( 'NONE',  ( 1.891708078845685481, -49.56698729999997255, -95.99999999890751212 ) ) ;
#8154 = DIRECTION ( 'NONE',  ( -0.7071067811865587860, 0.000000000000000000, -0.7071067811865362485 ) ) ;
#8155 = DIRECTION ( 'NONE',  ( 0.000000000000000000, 1.000000000000000000, 0.000000000000000000 ) ) ;
#8156 = ORIENTED_EDGE ( 'NONE', *, *, #803, .F. ) ;
#8157 = CARTESIAN_POINT ( 'NONE',  ( -31.39812190974910422, -49.95000000000000995, 8.827394325379140483 ) ) ;
#8158 = CARTESIAN_POINT ( 'NONE',  ( -38.46456197978948666, -32.40000000000000568, 4.312909747525784709 ) ) ;
#8159 = VERTEX_POINT ( 'NONE', #883 ) ;
#8160 = CARTESIAN_POINT ( 'NONE',  ( -34.99999999999997868, -45.00000000000000000, 30.00000000000000000 ) ) ;
#8161 = CARTESIAN_POINT ( 'NONE',  ( 1.891708078845685481, -49.56698729999997255, -98.39999999890753202 ) ) ;
#8162 = CARTESIAN_POINT ( 'NONE',  ( 5.000000000000000000, -47.07106781186545419, -96.14999999781504414 ) ) ;
#8163 = CARTESIAN_POINT ( 'NONE',  ( 2.071067811865477282, -49.99999999999997158, -97.84999999781504698 ) ) ;
#8164 = CARTESIAN_POINT ( 'NONE',  ( 3.229347689422841228, -48.22934768942280925, -99.74999999890752633 ) ) ;
#8165 = CARTESIAN_POINT ( 'NONE',  ( -41.99999999999996447, 48.00000000000002842, 20.35000000000000142 ) ) ;
#8166 = CARTESIAN_POINT ( 'NONE',  ( -38.38706344316003793, -43.70140427513058512, -1.382017864820032083 ) ) ;
#8167 = CARTESIAN_POINT ( 'NONE',  ( 4.999999999999998224, -42.92893218813448897, -95.34999999999999432 ) ) ;
#8168 = CARTESIAN_POINT ( 'NONE',  ( -34.05750781543319050, -42.15000000000000568, -7.963307464738194952 ) ) ;
#8169 = AXIS2_PLACEMENT_3D ( 'NONE', #1780, #7769, #6400 ) ;
#8170 = EDGE_CURVE ( 'NONE', #4354, #4208, #6617, .T. ) ;
#8171 = DIRECTION ( 'NONE',  ( -1.000000000000000000, 0.000000000000000000, 0.000000000000000000 ) ) ;
#8172 = EDGE_LOOP ( 'NONE', ( #994, #7071 ) ) ;
#8173 = CARTESIAN_POINT ( 'NONE',  ( 2.000000000000000000, 0.000000000000000000, 0.000000000000000000 ) ) ;
#8174 = CARTESIAN_POINT ( 'NONE',  ( -37.06321265474346660, -50.24999999999998579, 7.063212654743582952 ) ) ;
#8175 = CARTESIAN_POINT ( 'NONE',  ( -31.32969295284206979, -33.30000000000000426, -8.395350895058669494 ) ) ;
#8176 = VECTOR ( 'NONE', #938, 1000.000000000000000 ) ;
#8177 = CARTESIAN_POINT ( 'NONE',  ( -29.34127574812924522, -40.04081516742419922, 12.48372095990571573 ) ) ;
#8178 = CARTESIAN_POINT ( 'NONE',  ( -41.99999999999996447, 60.00000000000002842, -23.64999999999999858 ) ) ;
#8179 = CARTESIAN_POINT ( 'NONE',  ( -38.44051085762733777, -48.39859572486944472, 4.360112732550414982 ) ) ;
#8180 = EDGE_CURVE ( 'NONE', #772, #1675, #1982, .T. ) ;
#8181 = LINE ( 'NONE', #4872, #8029 ) ;
#8182 = CARTESIAN_POINT ( 'NONE',  ( -33.35889894354067309, 8.000000000000000000, -23.99999999999999289 ) ) ;
#8183 = SURFACE_SIDE_STYLE ('',( #4782 ) ) ;
#8184 = ORIENTED_EDGE ( 'NONE', *, *, #6788, .T. ) ;
#8185 = CARTESIAN_POINT ( 'NONE',  ( 42.00000000000000711, 60.00000000000002842, -23.64999999999992042 ) ) ;
#8186 = EDGE_LOOP ( 'NONE', ( #8690, #7788, #5718, #3468 ) ) ;
#8187 = CARTESIAN_POINT ( 'NONE',  ( -33.85891924778610473, -47.10000000000000142, 7.573555455601171715 ) ) ;
#8188 = CARTESIAN_POINT ( 'NONE',  ( -25.73429323749904185, -43.59859572486944046, -8.488613101951701267 ) ) ;
#8189 = CARTESIAN_POINT ( 'NONE',  ( -28.38237549136062654, -38.45140427513057801, -9.857197362228843573 ) ) ;
#8190 = CIRCLE ( 'NONE', #706, 1.000000000000000888 ) ;
#8191 = EDGE_LOOP ( 'NONE', ( #4141, #6163, #398, #4565 ) ) ;
#8192 = ORIENTED_EDGE ( 'NONE', *, *, #1854, .T. ) ;
#8193 = CARTESIAN_POINT ( 'NONE',  ( 4.566987299999998307, -43.10829192115428299, -96.39999999890753202 ) ) ;
#8194 = CARTESIAN_POINT ( 'NONE',  ( 30.00000000000001421, -44.99999999999995737, 30.00000000000000000 ) ) ;
#8195 = DIRECTION ( 'NONE',  ( -1.000000000000000000, 0.000000000000000000, 0.000000000000000000 ) ) ;
#8196 = CARTESIAN_POINT ( 'NONE',  ( -1.891708078845683483, -49.56698729999997255, -96.09999999890750644 ) ) ;
#8197 = LINE ( 'NONE', #2776, #2318 ) ;
#8198 = DIRECTION ( 'NONE',  ( -1.000000000000000000, 0.000000000000000000, -0.000000000000000000 ) ) ;
#8199 = EDGE_CURVE ( 'NONE', #2072, #2540, #7052, .T. ) ;
#8200 = ORIENTED_EDGE ( 'NONE', *, *, #1018, .T. ) ;
#8201 = PRESENTATION_LAYER_ASSIGNMENT (  '', '', ( #302 ) ) ;
#8202 = CARTESIAN_POINT ( 'NONE',  ( -25.89286002894218086, -35.64859572486943051, 7.938018618334153231 ) ) ;
#8203 = CARTESIAN_POINT ( 'NONE',  ( -28.43739315969223824, -33.45000000000000995, -9.865911304835512041 ) ) ;
#8204 = VERTEX_POINT ( 'NONE', #1636 ) ;
#8205 = CARTESIAN_POINT ( 'NONE',  ( -38.90016716647221529, -47.85000000000000853, -4.534861676072185155 ) ) ;
#8206 = CARTESIAN_POINT ( 'NONE',  ( 0.000000000000000000, 0.000000000000000000, 0.000000000000000000 ) ) ;
#8207 = CARTESIAN_POINT ( 'NONE',  ( 4.566987299999998307, -44.99999999999997158, -98.24999999890751212 ) ) ;
#8208 = CARTESIAN_POINT ( 'NONE',  ( 1.932551333443697450, -39.99999999999997158, -100.7466559142068832 ) ) ;
#8209 = DIRECTION ( 'NONE',  ( 0.000000000000000000, -0.5000000000000012212, -0.8660254037844380415 ) ) ;
#8210 = CARTESIAN_POINT ( 'NONE',  ( -4.566987299999997418, -46.89170807884566727, -99.19999999890751496 ) ) ;
#8211 = AXIS2_PLACEMENT_3D ( 'NONE', #1672, #4362, #2683 ) ;
#8212 = CARTESIAN_POINT ( 'NONE',  ( -21.61293655684001536, -42.20140427513058512, 1.382017864820032971 ) ) ;
#8213 = AXIS2_PLACEMENT_3D ( 'NONE', #2918, #8252, #4982 ) ;
#8214 = CARTESIAN_POINT ( 'NONE',  ( 2.071067811865477282, -49.99999999999996447, -95.54999999999999716 ) ) ;
#8215 = TOROIDAL_SURFACE ( 'NONE', #737, 2.200000000000001066, 0.2000000000000000111 ) ;
#8216 = CARTESIAN_POINT ( 'NONE',  ( -3.229347689422839451, -48.22934768942280925, -95.94999999890752918 ) ) ;
#8217 = CARTESIAN_POINT ( 'NONE',  ( -37.57355545560112375, -44.40000000000000568, 3.858919247786223305 ) ) ;
#8218 = LINE ( 'NONE', #1499, #2013 ) ;
#8219 = SHAPE_DEFINITION_REPRESENTATION ( #5076, #7373 ) ;
#8220 = ORIENTED_EDGE ( 'NONE', *, *, #1854, .F. ) ;
#8221 = PLANE ( 'NONE',  #4821 ) ;
#8222 = DIRECTION ( 'NONE',  ( 1.000000000000000000, 0.000000000000000000, 0.000000000000000000 ) ) ;
#8223 = CARTESIAN_POINT ( 'NONE',  ( -37.57355545560112375, -35.40000000000000568, 3.858919247786223305 ) ) ;
#8224 = AXIS2_PLACEMENT_3D ( 'NONE', #3780, #6458, #5801 ) ;
#8225 = CARTESIAN_POINT ( 'NONE',  ( -25.16324943048945073, -43.69086006543231804, 11.52652666073313092 ) ) ;
#8226 = CARTESIAN_POINT ( 'NONE',  ( 30.00000000000001421, -44.99999999999995737, -30.00100000000000122 ) ) ;
#8227 = CARTESIAN_POINT ( 'NONE',  ( -28.49241082802385350, -43.44859572486944188, -9.874625247442173404 ) ) ;
#8228 = ORIENTED_EDGE ( 'NONE', *, *, #7448, .T. ) ;
#8229 = CARTESIAN_POINT ( 'NONE',  ( 25.00000000000004263, -44.99999999999995737, -30.00100000000000122 ) ) ;
#8230 = EDGE_LOOP ( 'NONE', ( #7388, #3638, #8200, #4005 ) ) ;
#8231 = CARTESIAN_POINT ( 'NONE',  ( -28.65689575858256077, -40.44859572486944188, -8.836108267985801845 ) ) ;
#8232 = CARTESIAN_POINT ( 'NONE',  ( -22.97617564697422665, -37.74859572486943904, -7.102600956461224690 ) ) ;
#8233 = CARTESIAN_POINT ( 'NONE',  ( -34.48522952044771017, -44.15140427513058086, -8.925456012876139766 ) ) ;
#8234 = EDGE_CURVE ( 'NONE', #6235, #5482, #8302, .T. ) ;
#8235 = VECTOR ( 'NONE', #3166, 1000.000000000000000 ) ;
#8236 = EDGE_LOOP ( 'NONE', ( #3597, #3342, #3723, #2367 ) ) ;
#8237 = CARTESIAN_POINT ( 'NONE',  ( 4.566987300000000083, -46.89170807884564596, -96.49999999890755475 ) ) ;
#8238 = CARTESIAN_POINT ( 'NONE',  ( -4.999999999999987566, -42.92893218813447476, -99.84999999999999432 ) ) ;
#8239 = CYLINDRICAL_SURFACE ( 'NONE', #5162, 1.000000000000000888 ) ;
#8240 = CARTESIAN_POINT ( 'NONE',  ( -4.566987299999998307, -44.99999999999997158, -98.64999999890751781 ) ) ;
#8241 = CARTESIAN_POINT ( 'NONE',  ( 42.00000000000000711, 48.00000000000002842, -23.64999999999992042 ) ) ;
#8242 = CYLINDRICAL_SURFACE ( 'NONE', #4596, 4.999999999999998224 ) ;
#8243 =( BOUNDED_CURVE ( )  B_SPLINE_CURVE ( 2, ( #2571, #5329, #8031, #5244, #6039, #3365, #8078, #2524, #7942 ),
 .UNSPECIFIED., .F., .T. ) 
 B_SPLINE_CURVE_WITH_KNOTS ( ( 3, 2, 2, 2, 3 ),
 ( 0.4285714285714286031, 0.4464285714285715079, 0.4642857142857143016, 0.4821428571428571508, 0.5000000000000000000 ),
 .UNSPECIFIED. ) 
 CURVE ( )  GEOMETRIC_REPRESENTATION_ITEM ( )  RATIONAL_B_SPLINE_CURVE ( ( 0.9999999999999997780, 0.9238795325112869605, 1.000000000000000000, 0.9238795325112867385, 1.000000000000000000, 0.9238795325112867385, 1.000000000000000000, 0.9238795325112867385, 1.000000000000000000 ) ) 
 REPRESENTATION_ITEM ( '' )  );
#8244 = EDGE_LOOP ( 'NONE', ( #5356, #2189, #436, #6545 ) ) ;
#8245 = CARTESIAN_POINT ( 'NONE',  ( -31.32969295284206979, -48.30000000000001137, -8.395350895058669494 ) ) ;
#8246 = CARTESIAN_POINT ( 'NONE',  ( -39.38303923565386100, -32.70000000000000995, -1.486127417882099788 ) ) ;
#8247 = ORIENTED_EDGE ( 'NONE', *, *, #4757, .F. ) ;
#8248 = CARTESIAN_POINT ( 'NONE',  ( -22.93678734525658314, -45.74999999999999289, -7.063212654743582952 ) ) ;
#8249 = CARTESIAN_POINT ( 'NONE',  ( 5.000000000000004441, -47.07106781186543998, -98.54999999781504982 ) ) ;
#8250 = CARTESIAN_POINT ( 'NONE',  ( 8.389419568037416259E-16, -49.56698729999997255, -100.0499999989075093 ) ) ;
#8251 = CARTESIAN_POINT ( 'NONE',  ( -4.999999999999997335, -47.07106781186546129, -100.4499999978150413 ) ) ;
#8252 = DIRECTION ( 'NONE',  ( -0.000000000000000000, -0.000000000000000000, -1.000000000000000000 ) ) ;
#8253 = CARTESIAN_POINT ( 'NONE',  ( 1.891708078845682595, -40.43301269999998482, -98.69999999890752918 ) ) ;
#8254 = EDGE_CURVE ( 'NONE', #2617, #3764, #2352, .T. ) ;
#8255 = CARTESIAN_POINT ( 'NONE',  ( -22.06198138166579170, -45.35140427513057659, 4.107139971057695682 ) ) ;
#8256 = VECTOR ( 'NONE', #5905, 1000.000000000000000 ) ;
#8257 = CARTESIAN_POINT ( 'NONE',  ( -4.999999999999998224, -44.99999999999997158, -99.79300000002184845 ) ) ;
#8258 = CARTESIAN_POINT ( 'NONE',  ( 8.389419568037416259E-16, -49.56698729999997255, -96.64999999890753202 ) ) ;
#8259 = CARTESIAN_POINT ( 'NONE',  ( -21.60464910494133406, -46.20000000000000284, 1.329692952841886155 ) ) ;
#8260 = CARTESIAN_POINT ( 'NONE',  ( -4.783493649999997821, -44.99999999999997158, -95.12499999945376317 ) ) ;
#8261 = CONTEXT_DEPENDENT_SHAPE_REPRESENTATION ( #755, #7726 ) ;
#8262 = CARTESIAN_POINT ( 'NONE',  ( 2.071067811865477282, -49.99999999999997158, -100.2499999978150527 ) ) ;
#8263 = CARTESIAN_POINT ( 'NONE',  ( -26.14108075221394856, -42.60000000000000853, -7.573555455601170827 ) ) ;
#8264 = CARTESIAN_POINT ( 'NONE',  ( 19.99999999999997513, 1.224646799147352901E-14, 80.00000000000002842 ) ) ;
#8265 = CIRCLE ( 'NONE', #496, 0.5000000000000001110 ) ;
#8266 = PLANE ( 'NONE',  #7744 ) ;
#8267 = CARTESIAN_POINT ( 'NONE',  ( -25.41550616830297571, -47.64859572486945183, 8.874878320068054549 ) ) ;
#8268 = CARTESIAN_POINT ( 'NONE',  ( 30.00000000000000000, 60.00000000000002842, -1.102182119232617753E-14 ) ) ;
#8269 = CARTESIAN_POINT ( 'NONE',  ( -2.071067811865475505, -49.99999999999997158, -99.54999999781504982 ) ) ;
#8270 = EDGE_LOOP ( 'NONE', ( #2811, #2937, #8626, #7260 ) ) ;
#8271 = PLANE ( 'NONE',  #7131 ) ;
#8272 = ORIENTED_EDGE ( 'NONE', *, *, #6729, .T. ) ;
#8273 = CARTESIAN_POINT ( 'NONE',  ( -22.45049566656107842, -43.89859572486944472, -3.906122232810846917 ) ) ;
#8274 = CARTESIAN_POINT ( 'NONE',  ( -39.39132668755255651, -45.69859572486943478, -1.433802505903950308 ) ) ;
#8275 = CARTESIAN_POINT ( 'NONE',  ( -21.16389173201424612, -30.05140427513057944, -1.343104241417630185 ) ) ;
#8276 = VECTOR ( 'NONE', #728, 1000.000000000000000 ) ;
#8277 = CONICAL_SURFACE ( 'NONE', #4464, 1.610000000000000098, 0.7853981633974652654 ) ;
#8278 = EDGE_LOOP ( 'NONE', ( #1771, #7099, #6895, #7499 ) ) ;
#8279 = CARTESIAN_POINT ( 'NONE',  ( -4.566987299999998307, -43.10829192115428299, -100.0999999989075349 ) ) ;
#8280 = VECTOR ( 'NONE', #4226, 1000.000000000000000 ) ;
#8281 = CARTESIAN_POINT ( 'NONE',  ( -36.71751442127229836, -30.00000000000000711, -6.717514421272142044 ) ) ;
#8282 = FACE_OUTER_BOUND ( 'NONE', #6744, .T. ) ;
#8283 = CARTESIAN_POINT ( 'NONE',  ( 3.229347689422841228, -48.22934768942280925, -99.14999999890751781 ) ) ;
#8284 = CARTESIAN_POINT ( 'NONE',  ( -25.66707447546774645, -47.51618826727541034, 11.72657454140207456 ) ) ;
#8285 = FACE_OUTER_BOUND ( 'NONE', #4926, .T. ) ;
#8286 = ORIENTED_EDGE ( 'NONE', *, *, #7605, .F. ) ;
#8287 = EDGE_CURVE ( 'NONE', #8357, #1209, #4329, .T. ) ;
#8288 = CARTESIAN_POINT ( 'NONE',  ( -31.34310424141748896, -41.94859572486944188, 8.836108267985801845 ) ) ;
#8289 = CARTESIAN_POINT ( 'NONE',  ( -31.56260684030781505, -43.95000000000000284, 9.865911304835510265 ) ) ;
#8290 = VERTEX_POINT ( 'NONE', #5778 ) ;
#8291 = CARTESIAN_POINT ( 'NONE',  ( -34.31290974752564438, -50.10000000000000853, 8.464561979789547053 ) ) ;
#8292 = CARTESIAN_POINT ( 'NONE',  ( 0.1999999999999987899, 4.286263797015736595E-16, -3.500000000000000000 ) ) ;
#8293 = CARTESIAN_POINT ( 'NONE',  ( 1.891708078845685481, -49.56698729999997255, -99.99999999890751212 ) ) ;
#8294 = CARTESIAN_POINT ( 'NONE',  ( -3.535533905932735532, -48.53553390593270933, -97.99999999781503845 ) ) ;
#8295 = CARTESIAN_POINT ( 'NONE',  ( 2.000000000000000000, 0.000000000000000000, 0.000000000000000000 ) ) ;
#8296 = CARTESIAN_POINT ( 'NONE',  ( -1.891708078845683039, -40.43301269999998482, -99.39999999890751781 ) ) ;
#8297 = ORIENTED_EDGE ( 'NONE', *, *, #771, .T. ) ;
#8298 = CARTESIAN_POINT ( 'NONE',  ( -26.09387776718931917, -47.60140427513058370, -7.549504333439021941 ) ) ;
#8299 = CARTESIAN_POINT ( 'NONE',  ( -2.071067811865475061, -39.99999999999997158, -98.34300000002185982 ) ) ;
#8300 = CARTESIAN_POINT ( 'NONE',  ( 3.229347689422839895, -41.77065231057713390, -95.54999999890752349 ) ) ;
#8301 = CARTESIAN_POINT ( 'NONE',  ( -2.071067811865475505, -49.99999999999996447, -97.14999999781504414 ) ) ;
#8302 = LINE ( 'NONE', #2264, #6906 ) ;
#8303 = EDGE_CURVE ( 'NONE', #5475, #5184, #1681, .T. ) ;
#8304 = ITEM_DEFINED_TRANSFORMATION ( 'NONE', 'NONE', #307,  #2554 ) ;
#8305 = CARTESIAN_POINT ( 'NONE',  ( -30.00000000000002487, 0.000000000000000000, -29.65000000000000213 ) ) ;
#8306 = CARTESIAN_POINT ( 'NONE',  ( -21.17260567462091458, -43.04999999999999005, -1.398121909749242331 ) ) ;
#8307 = CARTESIAN_POINT ( 'NONE',  ( 0.000000000000000000, -44.99999999999997158, -95.00000000000000000 ) ) ;
#8308 = DIRECTION ( 'NONE',  ( 0.000000000000000000, 0.000000000000000000, -1.000000000000000000 ) ) ;
#8309 = CARTESIAN_POINT ( 'NONE',  ( -36.75497492228666374, -51.99859572486943193, -6.680053920257780220 ) ) ;
#8310 = CARTESIAN_POINT ( 'NONE',  ( -43.73819270004214843, -44.99999999999997158, 0.000000000000000000 ) ) ;
#8311 = CARTESIAN_POINT ( 'NONE',  ( -28.43739315969223824, -39.45000000000000284, -9.865911304835512041 ) ) ;
#8312 =( REPRESENTATION_RELATIONSHIP ('NONE','NONE', #2265, #6809 ) REPRESENTATION_RELATIONSHIP_WITH_TRANSFORMATION ( #1500 )SHAPE_REPRESENTATION_RELATIONSHIP( ) );
#8313 = EDGE_LOOP ( 'NONE', ( #8481, #3784, #6977, #4136 ) ) ;
#8314 = DIRECTION ( 'NONE',  ( 1.000000000000000000, -0.000000000000000000, -0.000000000000000000 ) ) ;
#8315 = EDGE_LOOP ( 'NONE', ( #5025, #8455, #4253, #4919 ) ) ;
#8316 = CARTESIAN_POINT ( 'NONE',  ( -31.34310424141748896, -41.94859572486944188, 8.836108267985801845 ) ) ;
#8317 = CARTESIAN_POINT ( 'NONE',  ( -37.02382435302582309, -48.24859572486943904, 7.102600956461226467 ) ) ;
#8318 = CARTESIAN_POINT ( 'NONE',  ( -23.64089511245930098, -29.75140427513057517, -6.280328284105564762 ) ) ;
#8319 = AXIS2_PLACEMENT_3D ( 'NONE', #4282, #1680, #6591 ) ;
#8320 = CARTESIAN_POINT ( 'NONE',  ( -4.566987299999997418, -46.89170807884566017, -96.79999999890752349 ) ) ;
#8321 = CARTESIAN_POINT ( 'NONE',  ( -7.654042494670954648E-16, -39.99999999999997158, -100.0000000000000000 ) ) ;
#8322 = DIRECTION ( 'NONE',  ( -1.000000000000000000, 0.000000000000000000, 0.000000000000000000 ) ) ;
#8323 = CARTESIAN_POINT ( 'NONE',  ( 1.891708078845682595, -40.43301269999998482, -98.89999999890751781 ) ) ;
#8324 = DIRECTION ( 'NONE',  ( 0.000000000000000000, 0.000000000000000000, -1.000000000000000000 ) ) ;
#8325 = DIRECTION ( 'NONE',  ( 0.000000000000000000, 0.000000000000000000, 1.000000000000000000 ) ) ;
#8326 = ORIENTED_EDGE ( 'NONE', *, *, #5608, .F. ) ;
#8327 = CARTESIAN_POINT ( 'NONE',  ( -23.95213185889994989, -38.49859572486943904, 5.972947139071243861 ) ) ;
#8328 = CARTESIAN_POINT ( 'NONE',  ( -39.38303923565386100, -44.70000000000000284, -1.486127417882099788 ) ) ;
#8329 = ORIENTED_EDGE ( 'NONE', *, *, #4797, .F. ) ;
#8330 = CARTESIAN_POINT ( 'NONE',  ( -25.63988726744978663, -29.60140427513057659, -8.440510857627391061 ) ) ;
#8331 =( NAMED_UNIT ( * ) SI_UNIT ( $, .STERADIAN. ) SOLID_ANGLE_UNIT ( ) );
#8332 = CARTESIAN_POINT ( 'NONE',  ( -4.566987299999998307, -43.10829192115428299, -100.2999999989075093 ) ) ;
#8333 = CARTESIAN_POINT ( 'NONE',  ( -3.535533905932736864, -41.46446609406723383, -98.19999999781505551 ) ) ;
#8334 = STYLED_ITEM ( 'NONE', ( #6485 ), #7808 ) ;
#8335 = DIRECTION ( 'NONE',  ( -0.000000000000000000, 1.000000000000000000, -0.000000000000000000 ) ) ;
#8336 = CARTESIAN_POINT ( 'NONE',  ( 3.229347689422839895, -41.77065231057713390, -97.14999999890753202 ) ) ;
#8337 = VERTEX_POINT ( 'NONE', #6307 ) ;
#8338 = CARTESIAN_POINT ( 'NONE',  ( -28.67030704715798350, -34.80000000000000426, 8.395350895058669494 ) ) ;
#8339 = CARTESIAN_POINT ( 'NONE',  ( -21.59636165304264921, -32.19859572486942767, 1.277368040863740228 ) ) ;
#8340 = EDGE_CURVE ( 'NONE', #8204, #8403, #6760, .T. ) ;
#8341 = CARTESIAN_POINT ( 'NONE',  ( -4.999999999999998224, -42.92893218813448897, -99.84300000002184561 ) ) ;
#8342 = DIRECTION ( 'NONE',  ( 1.000000000000000000, 0.000000000000000000, 0.000000000000000000 ) ) ;
#8343 = CARTESIAN_POINT ( 'NONE',  ( 2.071067811865477282, -49.99999999999996447, -96.24999999781505267 ) ) ;
#8344 = CONICAL_SURFACE ( 'NONE', #439, 1.535500000000000087, 1.047197551196590748 ) ;
#8345 = DIRECTION ( 'NONE',  ( 1.000000000000000000, 0.000000000000000000, 0.000000000000000000 ) ) ;
#8346 = EDGE_CURVE ( 'NONE', #7944, #4956, #157, .T. ) ;
#8347 = SURFACE_SIDE_STYLE ('',( #4865 ) ) ;
#8348 = CARTESIAN_POINT ( 'NONE',  ( -23.98959235991431171, -37.50000000000000711, 6.010407640085604797 ) ) ;
#8349 = CIRCLE ( 'NONE', #5522, 1.649999999999998579 ) ;
#8350 = ADVANCED_FACE ( 'NONE', ( #6348 ), #5734, .F. ) ;
#8351 = DIRECTION ( 'NONE',  ( 1.000000000000000000, 0.000000000000000000, 0.000000000000000000 ) ) ;
#8352 = DIRECTION ( 'NONE',  ( 0.000000000000000000, 0.000000000000000000, 1.000000000000000000 ) ) ;
#8353 = CARTESIAN_POINT ( 'NONE',  ( -21.09983283352784156, -37.35000000000000853, 4.534861676072186043 ) ) ;
#8354 = CARTESIAN_POINT ( 'NONE',  ( 2.000000000000000000, -0.8865213383406729264, -1.535499999999999421 ) ) ;
#8355 = CARTESIAN_POINT ( 'NONE',  ( -38.46456197978948666, -44.40000000000000568, 4.312909747525784709 ) ) ;
#8356 = SURFACE_STYLE_USAGE ( .BOTH. , #4383 ) ;
#8357 = VERTEX_POINT ( 'NONE', #6392 ) ;
#8358 = DIRECTION ( 'NONE',  ( 0.000000000000000000, 0.000000000000000000, 1.000000000000000000 ) ) ;
#8359 = ORIENTED_EDGE ( 'NONE', *, *, #6398, .F. ) ;
#8360 = AXIS2_PLACEMENT_3D ( 'NONE', #7697, #3644, #161 ) ;
#8361 = CARTESIAN_POINT ( 'NONE',  ( -28.61798213517984024, -41.79859572486943620, 8.387063443159973986 ) ) ;
#8362 = CARTESIAN_POINT ( 'NONE',  ( -36.75497492228666374, -45.99859572486943904, -6.680053920257780220 ) ) ;
#8363 = CARTESIAN_POINT ( 'NONE',  ( -38.48861310195163554, -46.40140427513058086, 4.265706762501153548 ) ) ;
#8364 = CARTESIAN_POINT ( 'NONE',  ( 3.229347689422839895, -41.77065231057713390, -97.14999999890753202 ) ) ;
#8365 = VECTOR ( 'NONE', #8622, 1000.000000000000000 ) ;
#8366 = DIRECTION ( 'NONE',  ( 0.000000000000000000, -0.5000000000000011102, -0.8660254037844379305 ) ) ;
#8367 = CARTESIAN_POINT ( 'NONE',  ( -31.56260684030781505, -31.95000000000000639, 9.865911304835510265 ) ) ;
#8368 = PRODUCT_DEFINITION_SHAPE ( 'NONE', 'NONE',  #8733 ) ;
#8369 = CARTESIAN_POINT ( 'NONE',  ( 4.566987300000000083, -46.89170807884565306, -97.49999999890754054 ) ) ;
#8370 = FACE_OUTER_BOUND ( 'NONE', #3578, .T. ) ;
#8371 = CARTESIAN_POINT ( 'NONE',  ( 1.891708078845685481, -49.56698729999997255, -96.79999999890753770 ) ) ;
#8372 = ORIENTED_EDGE ( 'NONE', *, *, #2126, .T. ) ;
#8373 = CARTESIAN_POINT ( 'NONE',  ( -38.81868038277247734, -39.54859572486944330, 1.453139578080855365 ) ) ;
#8374 = EDGE_CURVE ( 'NONE', #3309, #4035, #3260, .T. ) ;
#8375 = VECTOR ( 'NONE', #7203, 1000.000000000000000 ) ;
#8376 = CARTESIAN_POINT ( 'NONE',  ( -28.51387258211773812, -40.80000000000000426, 9.383039235653802379 ) ) ;
#8377 = ADVANCED_FACE ( 'NONE', ( #1731, #4416 ), #390, .F. ) ;
#8378 = EDGE_LOOP ( 'NONE', ( #1254, #1801, #1604, #1558 ) ) ;
#8379 = CARTESIAN_POINT ( 'NONE',  ( -25.68709025247441602, -45.60000000000000853, -8.464561979789547053 ) ) ;
#8380 = DIRECTION ( 'NONE',  ( 1.000000000000000000, -0.000000000000000000, -0.000000000000000000 ) ) ;
#8381 = CARTESIAN_POINT ( 'NONE',  ( -3.061616997868382155E-16, -39.99999999999997158, -100.0624999997268958 ) ) ;
#8382 = CARTESIAN_POINT ( 'NONE',  ( -4.999999999999998224, -42.92893218813448897, -99.74999999781503845 ) ) ;
#8383 = DIRECTION ( 'NONE',  ( -0.000000000000000000, -0.000000000000000000, -1.000000000000000000 ) ) ;
#8384 = CARTESIAN_POINT ( 'NONE',  ( -4.999999999999998224, -42.92893218813448897, -96.64999999999999147 ) ) ;
#8385 = ORIENTED_EDGE ( 'NONE', *, *, #6003, .T. ) ;
#8386 = CARTESIAN_POINT ( 'NONE',  ( -38.82739432537914581, -32.55000000000000426, 1.398121909749243441 ) ) ;
#8387 = ORIENTED_EDGE ( 'NONE', *, *, #1055, .T. ) ;
#8388 = UNCERTAINTY_MEASURE_WITH_UNIT (LENGTH_MEASURE( 1.000000000000000082E-05 ), #4077, 'distance_accuracy_value', 'NONE');
#8389 = CARTESIAN_POINT ( 'NONE',  ( -4.566987299999998307, -44.99999999999997158, -96.04999999890752349 ) ) ;
#8390 = CARTESIAN_POINT ( 'NONE',  ( -2.071067811865475061, -39.99999999999997158, -95.84999999781503277 ) ) ;
#8391 = DIRECTION ( 'NONE',  ( 0.000000000000000000, 0.000000000000000000, -1.000000000000000000 ) ) ;
#8392 = CARTESIAN_POINT ( 'NONE',  ( -45.00000000000003553, -44.99999999999997158, 2.099999999999997868 ) ) ;
#8393 = CARTESIAN_POINT ( 'NONE',  ( -28.67030704715798350, -37.80000000000000426, 8.395350895058669494 ) ) ;
#8394 = PRODUCT_DEFINITION_SHAPE ( 'NONE', 'NONE',  #1576 ) ;
#8395 = VECTOR ( 'NONE', #2558, 1000.000000000000114 ) ;
#8396 = CARTESIAN_POINT ( 'NONE',  ( -2.796473189345805913E-16, -40.43301269999997061, -95.64999999890753202 ) ) ;
#8397 = CARTESIAN_POINT ( 'NONE',  ( 0.000000000000000000, -44.99999999999997158, -105.0000000000000142 ) ) ;
#8398 = CARTESIAN_POINT ( 'NONE',  ( -37.06321265474346660, -35.24999999999998579, 7.063212654743582952 ) ) ;
#8399 = CARTESIAN_POINT ( 'NONE',  ( 25.00000000000004263, -44.99999999999995737, 11.45643923738958314 ) ) ;
#8400 = CARTESIAN_POINT ( 'NONE',  ( -39.86591130483550671, -41.55000000000000426, 1.562606840307984690 ) ) ;
#8401 = FILL_AREA_STYLE ('',( #5041 ) ) ;
#8402 = ORIENTED_EDGE ( 'NONE', *, *, #1574, .T. ) ;
#8403 = VERTEX_POINT ( 'NONE', #1187 ) ;
#8404 = CARTESIAN_POINT ( 'NONE',  ( -22.45049566656107842, -37.89859572486944472, -3.906122232810846917 ) ) ;
#8405 = CARTESIAN_POINT ( 'NONE',  ( -20.60867331244750034, -50.19859572486944188, 1.433802505903951419 ) ) ;
#8406 = CARTESIAN_POINT ( 'NONE',  ( -21.16389173201424612, -33.05140427513057233, -1.343104241417630185 ) ) ;
#8407 = CIRCLE ( 'NONE', #2779, 1.000000000000000888 ) ;
#8408 = CARTESIAN_POINT ( 'NONE',  ( 4.566987300000000083, -46.89170807884564596, -98.89999999890753202 ) ) ;
#8409 = DIRECTION ( 'NONE',  ( -0.000000000000000000, -0.000000000000000000, -1.000000000000000000 ) ) ;
#8410 = CARTESIAN_POINT ( 'NONE',  ( -39.38303923565386100, -38.70000000000000284, -1.486127417882099788 ) ) ;
#8411 = VECTOR ( 'NONE', #6409, 1000.000000000000000 ) ;
#8412 = CARTESIAN_POINT ( 'NONE',  ( 1.891708078845685481, -49.56698729999997255, -99.99999999890751212 ) ) ;
#8413 = DIRECTION ( 'NONE',  ( 1.000000000000000000, 0.000000000000000000, 0.000000000000000000 ) ) ;
#8414 = CARTESIAN_POINT ( 'NONE',  ( 1.891708078845685481, -49.56698729999997255, -97.59999999890754907 ) ) ;
#8415 =( NAMED_UNIT ( * ) SI_UNIT ( $, .STERADIAN. ) SOLID_ANGLE_UNIT ( ) );
#8416 = ORIENTED_EDGE ( 'NONE', *, *, #2490, .T. ) ;
#8417 = CARTESIAN_POINT ( 'NONE',  ( -38.81868038277247734, -42.54859572486944330, 1.453139578080855365 ) ) ;
#8418 = CARTESIAN_POINT ( 'NONE',  ( -31.48612741788231517, -42.30000000000000426, -9.383039235653804155 ) ) ;
#8419 = AXIS2_PLACEMENT_3D ( 'NONE', #49, #2753, #6000 ) ;
#8420 = EDGE_LOOP ( 'NONE', ( #1852, #7264, #6148, #4715 ) ) ;
#8421 = CARTESIAN_POINT ( 'NONE',  ( -21.12512167993187973, -33.35140427513057659, 4.584493831696868860 ) ) ;
#8422 = CARTESIAN_POINT ( 'NONE',  ( -3.535533905932736864, -41.46446609406723383, -96.59999999781504698 ) ) ;
#8423 = CARTESIAN_POINT ( 'NONE',  ( 4.999999999999998224, -44.99999999999997158, -95.00000000000000000 ) ) ;
#8424 = CARTESIAN_POINT ( 'NONE',  ( 2.071067811865477282, -49.99999999999997158, -95.54999999999999716 ) ) ;
#8425 = DIRECTION ( 'NONE',  ( 0.000000000000000000, 0.000000000000000000, 1.000000000000000000 ) ) ;
#8426 = CARTESIAN_POINT ( 'NONE',  ( -2.071067811865475061, -39.99999999999997158, -97.54999999999998295 ) ) ;
#8427 = ORIENTED_EDGE ( 'NONE', *, *, #6921, .T. ) ;
#8428 = CARTESIAN_POINT ( 'NONE',  ( -31.32969295284206979, -36.30000000000000426, -8.395350895058669494 ) ) ;
#8429 = VERTEX_POINT ( 'NONE', #1901 ) ;
#8430 = CARTESIAN_POINT ( 'NONE',  ( 3.535533905932737309, -48.53553390593270933, -98.70000000000000284 ) ) ;
#8431 = CARTESIAN_POINT ( 'NONE',  ( -36.31971658582311591, -50.24999999999999289, 6.319716585823200283 ) ) ;
#8432 = DIRECTION ( 'NONE',  ( 0.000000000000000000, 0.000000000000000000, 1.000000000000000000 ) ) ;
#8433 = CONTEXT_DEPENDENT_SHAPE_REPRESENTATION ( #7972, #8368 ) ;
#8434 = CARTESIAN_POINT ( 'NONE',  ( -45.00000000000003553, -44.99999999999997158, 0.000000000000000000 ) ) ;
#8435 = CARTESIAN_POINT ( 'NONE',  ( -33.85891924778610473, -44.10000000000000853, 7.573555455601171715 ) ) ;
#8436 = CARTESIAN_POINT ( 'NONE',  ( -4.999999999999998224, -42.92893218813449607, -99.74999999781503845 ) ) ;
#8437 = CARTESIAN_POINT ( 'NONE',  ( -26.64110105645932336, -7.999999999999996447, -23.99999999999999289 ) ) ;
#8438 = CARTESIAN_POINT ( 'NONE',  ( -31.32969295284206979, -30.30000000000000782, -8.395350895058669494 ) ) ;
#8439 = CARTESIAN_POINT ( 'NONE',  ( -38.46456197978948666, -32.40000000000000568, 4.312909747525784709 ) ) ;
#8440 = CARTESIAN_POINT ( 'NONE',  ( -44.14999999999995595, -22.00000000000000000, 80.00000000000002842 ) ) ;
#8441 = CARTESIAN_POINT ( 'NONE',  ( -28.43739315969223824, -36.44999999999999574, -9.865911304835512041 ) ) ;
#8442 = EDGE_CURVE ( 'NONE', #598, #5405, #3115, .T. ) ;
#8443 = CARTESIAN_POINT ( 'NONE',  ( 0.000000000000000000, 0.000000000000000000, 0.000000000000000000 ) ) ;
#8444 = EDGE_LOOP ( 'NONE', ( #8586, #3442, #681, #7733 ) ) ;
#8445 = CARTESIAN_POINT ( 'NONE',  ( -31.53845232986046554, -31.29859572486943975, -9.374751783755117529 ) ) ;
#8446 = CARTESIAN_POINT ( 'NONE',  ( -22.97617564697422665, -49.74859572486944614, -7.102600956461224690 ) ) ;
#8447 = CARTESIAN_POINT ( 'NONE',  ( -31.27736804086391942, -38.30140427513057944, -8.403638346957361449 ) ) ;
#8448 = EDGE_CURVE ( 'NONE', #1297, #1434, #7270, .T. ) ;
#8449 = CARTESIAN_POINT ( 'NONE',  ( 25.00000000000004263, -44.99999999999995737, 30.00000000000000000 ) ) ;
#8450 = CARTESIAN_POINT ( 'NONE',  ( 33.30788680089139575, -41.23645700522180846, 12.05676622698251776 ) ) ;
#8451 = CARTESIAN_POINT ( 'NONE',  ( -39.86591130483550671, -35.55000000000001137, 1.562606840307984468 ) ) ;
#8452 = CYLINDRICAL_SURFACE ( 'NONE', #7599, 7.499999999999999112 ) ;
#8453 = DIRECTION ( 'NONE',  ( 0.000000000000000000, 0.000000000000000000, 1.000000000000000000 ) ) ;
#8454 = AXIS2_PLACEMENT_3D ( 'NONE', #5651, #7014, #8352 ) ;
#8455 = ORIENTED_EDGE ( 'NONE', *, *, #6223, .T. ) ;
#8456 = CARTESIAN_POINT ( 'NONE',  ( 4.999999999999998224, -44.99999999999997158, -95.00000000000000000 ) ) ;
#8457 = CARTESIAN_POINT ( 'NONE',  ( -31.34310424141748896, -38.94859572486943478, 8.836108267985801845 ) ) ;
#8458 = CARTESIAN_POINT ( 'NONE',  ( -34.53486167607238144, -45.14999999999999858, -8.900167166472096270 ) ) ;
#8459 = ORIENTED_EDGE ( 'NONE', *, *, #3755, .T. ) ;
#8460 = CARTESIAN_POINT ( 'NONE',  ( -39.37475178375516549, -34.70140427513057091, -1.538452329860249712 ) ) ;
#8461 = AXIS2_PLACEMENT_3D ( 'NONE', #7465, #4954, #5520 ) ;
#8462 = CARTESIAN_POINT ( 'NONE',  ( 0.000000000000000000, -44.99999999999997158, -95.00000000000000000 ) ) ;
#8463 = FACE_OUTER_BOUND ( 'NONE', #7211, .T. ) ;
#8464 = EDGE_CURVE ( 'NONE', #7480, #2692, #3803, .T. ) ;
#8465 = DIRECTION ( 'NONE',  ( 0.000000000000000000, 0.000000000000000000, -1.000000000000000000 ) ) ;
#8466 = CARTESIAN_POINT ( 'NONE',  ( 2.000000000000000000, -0.8865213383406729264, -1.535499999999999421 ) ) ;
#8467 = CARTESIAN_POINT ( 'NONE',  ( -4.999999999999997335, -47.07106781186546129, -95.75000000000000000 ) ) ;
#8468 = EDGE_LOOP ( 'NONE', ( #8520, #2276 ) ) ;
#8469 = CARTESIAN_POINT ( 'NONE',  ( -28.60187809025093841, -33.45000000000000995, -8.827394325379140483 ) ) ;
#8470 = ORIENTED_EDGE ( 'NONE', *, *, #3384, .F. ) ;
#8471 = CARTESIAN_POINT ( 'NONE',  ( -3.535533905932736864, -41.46446609406723383, -96.70000000000000284 ) ) ;
#8472 = CARTESIAN_POINT ( 'NONE',  ( -3.535533905932736864, -41.46446609406723383, -96.59999999781504698 ) ) ;
#8473 = CARTESIAN_POINT ( 'NONE',  ( -30.00000000000019185, 0.000000000000000000, -41.34999999999999432 ) ) ;
#8474 = COLOUR_RGB ( '', 0.09019608, 0.27058824, 0.51372549) ;
#8475 = CARTESIAN_POINT ( 'NONE',  ( -4.999999999999998224, -44.99999999999997158, -97.40000000000000568 ) ) ;
#8476 = CARTESIAN_POINT ( 'NONE',  ( 3.535533969928884801, -41.46446615806338087, -100.0000000000000142 ) ) ;
#8477 = PRESENTATION_LAYER_ASSIGNMENT (  '', '', ( #722 ) ) ;
#8478 = FACE_OUTER_BOUND ( 'NONE', #1124, .T. ) ;
#8479 = CARTESIAN_POINT ( 'NONE',  ( -33.35889894354067309, 10.00000000000000178, -24.00000000000000000 ) ) ;
#8480 = CARTESIAN_POINT ( 'NONE',  ( -31.48612741788231517, -36.30000000000000426, -9.383039235653804155 ) ) ;
#8481 = ORIENTED_EDGE ( 'NONE', *, *, #2361, .T. ) ;
#8482 = CARTESIAN_POINT ( 'NONE',  ( -28.65689575858256077, -46.44859572486943478, -8.836108267985801845 ) ) ;
#8483 = CARTESIAN_POINT ( 'NONE',  ( -34.31290974752564438, -41.10000000000000142, 8.464561979789547053 ) ) ;
#8484 = AXIS2_PLACEMENT_3D ( 'NONE', #6868, #4318, #80 ) ;
#8485 = CARTESIAN_POINT ( 'NONE',  ( -22.40239342223677355, -38.90140427513058086, -3.811716262761597473 ) ) ;
#8486 = CARTESIAN_POINT ( 'NONE',  ( 3.229347689422841228, -48.22934768942280925, -98.14999999890753202 ) ) ;
#8487 = CARTESIAN_POINT ( 'NONE',  ( -26.64110105645932336, -8.999999999999998224, 124.0000000000000000 ) ) ;
#8488 = CARTESIAN_POINT ( 'NONE',  ( -20.61696076434619584, -34.20000000000000995, 1.486127417882100676 ) ) ;
#8489 = CARTESIAN_POINT ( 'NONE',  ( -3.229347689422839451, -48.22934768942280925, -99.34999999890752065 ) ) ;
#8490 = DIRECTION ( 'NONE',  ( 1.000000000000000000, -0.000000000000000000, -0.000000000000000000 ) ) ;
#8491 = AXIS2_PLACEMENT_3D ( 'NONE', #7838, #5106, #7797 ) ;
#8492 = CARTESIAN_POINT ( 'NONE',  ( -1.891708078845683039, -40.43301269999998482, -97.99999999890752633 ) ) ;
#8493 = CYLINDRICAL_SURFACE ( 'NONE', #2978, 4.999999999999998224 ) ;
#8494 = ORIENTED_EDGE ( 'NONE', *, *, #1630, .F. ) ;
#8495 = CARTESIAN_POINT ( 'NONE',  ( -25.64110105645932336, -7.999999999999996447, 124.0000000000000000 ) ) ;
#8496 = ADVANCED_FACE ( 'NONE', ( #8513 ), #7849, .F. ) ;
#8497 = CARTESIAN_POINT ( 'NONE',  ( -39.85719736222883824, -33.54859572486944330, 1.617624508639602388 ) ) ;
#8498 = CARTESIAN_POINT ( 'NONE',  ( -20.62524821624488069, -30.20140427513057446, 1.538452329860250378 ) ) ;
#8499 = CIRCLE ( 'NONE', #5822, 2.000000000000001776 ) ;
#8500 = VERTEX_POINT ( 'NONE', #7312 ) ;
#8501 = CARTESIAN_POINT ( 'NONE',  ( -39.87462524744216807, -40.55140427513058654, 1.507589171976367215 ) ) ;
#8502 = CARTESIAN_POINT ( 'NONE',  ( -33.05780150203954548, -48.96939036817698820, 12.12340239416035992 ) ) ;
#8503 = DIRECTION ( 'NONE',  ( -1.000000000000000000, 0.000000000000000000, 0.000000000000000000 ) ) ;
#8504 = DIRECTION ( 'NONE',  ( -0.000000000000000000, 1.000000000000000000, -0.000000000000000000 ) ) ;
#8505 = FACE_BOUND ( 'NONE', #2022, .T. ) ;
#8506 = CARTESIAN_POINT ( 'NONE',  ( -3.535533905932736864, -41.46446609406723383, -95.90000000000000568 ) ) ;
#8507 = VERTEX_POINT ( 'NONE', #3835 ) ;
#8508 = CARTESIAN_POINT ( 'NONE',  ( -24.02705286092866643, -48.50140427513058938, 6.047868141099968398 ) ) ;
#8509 = CIRCLE ( 'NONE', #8080, 11.99999999999983302 ) ;
#8510 = ORIENTED_EDGE ( 'NONE', *, *, #6522, .F. ) ;
#8511 = EDGE_CURVE ( 'NONE', #1675, #7794, #8190, .T. ) ;
#8512 = CARTESIAN_POINT ( 'NONE',  ( -3.061616997868382155E-16, -39.99999999999997158, -96.79999999999999716 ) ) ;
#8513 = FACE_OUTER_BOUND ( 'NONE', #8230, .T. ) ;
#8514 = DIRECTION ( 'NONE',  ( -0.000000000000000000, -0.000000000000000000, -1.000000000000000000 ) ) ;
#8515 = CARTESIAN_POINT ( 'NONE',  ( -34.35889894354067309, -7.999999999999996447, 124.0000000000000000 ) ) ;
#8516 = FACE_OUTER_BOUND ( 'NONE', #6026, .T. ) ;
#8517 = CYLINDRICAL_SURFACE ( 'NONE', #5199, 1.649999999999998579 ) ;
#8518 = CARTESIAN_POINT ( 'NONE',  ( -20.00000000000002487, 0.000000000000000000, -29.65000000000000213 ) ) ;
#8519 = CARTESIAN_POINT ( 'NONE',  ( -28.51387258211773812, -49.80000000000001137, 9.383039235653802379 ) ) ;
#8520 = ORIENTED_EDGE ( 'NONE', *, *, #4818, .F. ) ;
#8521 = CARTESIAN_POINT ( 'NONE',  ( -20.14280263777121149, -32.04859572486944330, -1.617624508639600833 ) ) ;
#8522 = CARTESIAN_POINT ( 'NONE',  ( -20.13408869516453947, -37.05000000000001137, -1.562606840307983136 ) ) ;
#8523 = CARTESIAN_POINT ( 'NONE',  ( -38.38706344316003793, -37.70140427513057091, -1.382017864820032083 ) ) ;
#8524 = EDGE_CURVE ( 'NONE', #3779, #6167, #5366, .T. ) ;
#8525 = CARTESIAN_POINT ( 'NONE',  ( -4.566987299999998307, -43.10829192115428299, -98.49999999890752633 ) ) ;
#8526 = DIRECTION ( 'NONE',  ( 1.000000000000000000, 0.000000000000000000, 0.000000000000000000 ) ) ;
#8527 = CARTESIAN_POINT ( 'NONE',  ( -31.50758917197619979, -35.94859572486944188, 9.874625247442176956 ) ) ;
#8528 = CARTESIAN_POINT ( 'NONE',  ( -36.71751442127229836, -33.00000000000000711, -6.717514421272142044 ) ) ;
#8529 = CARTESIAN_POINT ( 'NONE',  ( -1.891708078845683483, -49.56698729999997255, -99.29999999890752349 ) ) ;
#8530 = DIRECTION ( 'NONE',  ( 0.000000000000000000, 0.000000000000000000, -1.000000000000000000 ) ) ;
#8531 = CARTESIAN_POINT ( 'NONE',  ( 4.566987300000000083, -46.89170807884565306, -97.49999999890754054 ) ) ;
#8532 = AXIS2_PLACEMENT_3D ( 'NONE', #7008, #7623, #4281 ) ;
#8533 = SURFACE_STYLE_USAGE ( .BOTH. , #7831 ) ;
#8534 = ORIENTED_EDGE ( 'NONE', *, *, #3323, .F. ) ;
#8535 = CARTESIAN_POINT ( 'NONE',  ( -40.00000000000002842, 1.224646799147353059E-15, -28.65000000000000213 ) ) ;
#8536 = CARTESIAN_POINT ( 'NONE',  ( -36.04786814110010340, -51.99859572486943193, -5.972947139071243861 ) ) ;
#8537 = CARTESIAN_POINT ( 'NONE',  ( -38.48861310195163554, -34.40140427513058086, 4.265706762501153548 ) ) ;
#8538 = VERTEX_POINT ( 'NONE', #8165 ) ;
#8539 = ORIENTED_EDGE ( 'NONE', *, *, #7948, .T. ) ;
#8540 = CARTESIAN_POINT ( 'NONE',  ( -34.36011273255026310, -37.10140427513057659, 8.440510857627391061 ) ) ;
#8541 = CARTESIAN_POINT ( 'NONE',  ( -31.62616360386732950, -49.73950299483296078, 12.39754634550705603 ) ) ;
#8542 = CARTESIAN_POINT ( 'NONE',  ( -44.14999999999995595, 22.00000000000000000, 80.00000000000002842 ) ) ;
#8543 = CARTESIAN_POINT ( 'NONE',  ( -4.999999999999998224, -44.99999999999997158, -98.19999999999998863 ) ) ;
#8544 = EDGE_CURVE ( 'NONE', #6933, #1925, #849, .T. ) ;
#8545 = CARTESIAN_POINT ( 'NONE',  ( -30.00000000000002487, 0.000000000000000000, -29.65000000000000213 ) ) ;
#8546 = CARTESIAN_POINT ( 'NONE',  ( 3.535533905932736420, -41.46446609406723383, -97.69999999999998863 ) ) ;
#8547 = EDGE_LOOP ( 'NONE', ( #1323, #4466, #305, #6720 ) ) ;
#8548 = CARTESIAN_POINT ( 'NONE',  ( -38.82739432537914581, -44.55000000000001137, 1.398121909749243441 ) ) ;
#8549 = VECTOR ( 'NONE', #6443, 1000.000000000000000 ) ;
#8550 = VECTOR ( 'NONE', #1201, 1000.000000000000000 ) ;
#8551 = VERTEX_POINT ( 'NONE', #4970 ) ;
#8552 = PRODUCT_DEFINITION_CONTEXT ( 'detailed design', #6659, 'design' ) ;
#8553 = ADVANCED_FACE ( 'NONE', ( #4765 ), #7653, .T. ) ;
#8554 = CARTESIAN_POINT ( 'NONE',  ( -2.071067811865475061, -39.99999999999997158, -98.35000000000000853 ) ) ;
#8555 = CARTESIAN_POINT ( 'NONE',  ( 3.215378252671984072, -48.83965459759100725, -99.99931211326003222 ) ) ;
#8556 = CARTESIAN_POINT ( 'NONE',  ( -21.16389173201424612, -36.05140427513057944, -1.343104241417630185 ) ) ;
#8557 = FACE_OUTER_BOUND ( 'NONE', #6907, .T. ) ;
#8558 = CIRCLE ( 'NONE', #4058, 1.000000000000000888 ) ;
#8559 = CARTESIAN_POINT ( 'NONE',  ( -25.64110105645932336, 8.000000000000000000, -24.00000000000000000 ) ) ;
#8560 = CARTESIAN_POINT ( 'NONE',  ( -21.60464910494133406, -37.20000000000000284, 1.329692952841886155 ) ) ;
#8561 = ADVANCED_FACE ( 'NONE', ( #248 ), #2949, .T. ) ;
#8562 = CARTESIAN_POINT ( 'NONE',  ( -4.999999999999998224, -44.99999999999997158, -96.60000000000000853 ) ) ;
#8563 = CARTESIAN_POINT ( 'NONE',  ( 7.499999999999999112, -44.99999999999997158, -100.0000000000000000 ) ) ;
#8564 = ORIENTED_EDGE ( 'NONE', *, *, #4199, .T. ) ;
#8565 = CARTESIAN_POINT ( 'NONE',  ( -38.81868038277247734, -48.54859572486944330, 1.453139578080855365 ) ) ;
#8566 = CARTESIAN_POINT ( 'NONE',  ( -23.28248557872775137, -40.50000000000000711, 6.717514421272141156 ) ) ;
#8567 = CARTESIAN_POINT ( 'NONE',  ( -22.06198138166579170, -36.35140427513057659, 4.107139971057695682 ) ) ;
#8568 = CARTESIAN_POINT ( 'NONE',  ( -2.071067811865475061, -39.99999999999997158, -96.75000000000001421 ) ) ;
#8569 = FACE_OUTER_BOUND ( 'NONE', #2869, .T. ) ;
#8570 = CARTESIAN_POINT ( 'NONE',  ( -21.07454398712378918, -41.34859572486944757, 4.485229520447505003 ) ) ;
#8571 = CARTESIAN_POINT ( 'NONE',  ( -31.56260684030781505, -34.95000000000000995, 9.865911304835510265 ) ) ;
#8572 = DIRECTION ( 'NONE',  ( -0.000000000000000000, -0.000000000000000000, -1.000000000000000000 ) ) ;
#8573 = FACE_OUTER_BOUND ( 'NONE', #1225, .T. ) ;
#8574 = CARTESIAN_POINT ( 'NONE',  ( -1.891708078845683039, -40.43301269999998482, -99.59999999890754907 ) ) ;
#8575 = FILL_AREA_STYLE_COLOUR ( '', #6214 ) ;
#8576 = ORIENTED_EDGE ( 'NONE', *, *, #4546, .T. ) ;
#8577 = CARTESIAN_POINT ( 'NONE',  ( -31.53845232986046554, -34.29859572486943620, -9.374751783755117529 ) ) ;
#8578 = CARTESIAN_POINT ( 'NONE',  ( -28.51387258211773812, -49.80000000000001137, 9.383039235653802379 ) ) ;
#8579 = EDGE_LOOP ( 'NONE', ( #7193, #8329 ) ) ;
#8580 = ORIENTED_EDGE ( 'NONE', *, *, #3272, .T. ) ;
#8581 = CARTESIAN_POINT ( 'NONE',  ( -21.12512167993187973, -36.35140427513057659, 4.584493831696868860 ) ) ;
#8582 = CARTESIAN_POINT ( 'NONE',  ( 50.00000000000002842, -30.00000000000000000, 80.00000000000002842 ) ) ;
#8583 = DIRECTION ( 'NONE',  ( -0.000000000000000000, -0.000000000000000000, -1.000000000000000000 ) ) ;
#8584 = CARTESIAN_POINT ( 'NONE',  ( 34.96775378464300132, -45.65699184524252274, 11.47067790983490099 ) ) ;
#8585 = CARTESIAN_POINT ( 'NONE',  ( 2.071067811865477282, -49.99999999999996447, -99.54999999999998295 ) ) ;
#8586 = ORIENTED_EDGE ( 'NONE', *, *, #257, .T. ) ;
#8587 = APPLICATION_CONTEXT ( 'automotive_design' ) ;
#8588 = CARTESIAN_POINT ( 'NONE',  ( -36.31971658582311591, -44.25000000000000000, 6.319716585823199395 ) ) ;
#8589 = EDGE_CURVE ( 'NONE', #5405, #8551, #998, .T. ) ;
#8590 = VECTOR ( 'NONE', #4604, 1000.000000000000000 ) ;
#8591 = EDGE_CURVE ( 'NONE', #4124, #3192, #4941, .T. ) ;
#8592 = ORIENTED_EDGE ( 'NONE', *, *, #1148, .T. ) ;
#8593 = LINE ( 'NONE', #7977, #8395 ) ;
#8594 = CARTESIAN_POINT ( 'NONE',  ( 9.184850993605145972E-16, -49.99999999999997158, -96.40000000000000568 ) ) ;
#8595 = CARTESIAN_POINT ( 'NONE',  ( -20.61696076434619584, -40.20000000000000995, 1.486127417882100676 ) ) ;
#8596 = CARTESIAN_POINT ( 'NONE',  ( -2.796473189345805913E-16, -40.43301269999997061, -98.64999999890753202 ) ) ;
#8597 = CARTESIAN_POINT ( 'NONE',  ( -4.988661577999454089, -45.44142994503554434, -100.0006878868518783 ) ) ;
#8598 = CARTESIAN_POINT ( 'NONE',  ( -36.35910488754074521, -31.25140427513058228, 6.280328284105565650 ) ) ;
#8599 = EDGE_CURVE ( 'NONE', #4661, #94, #1985, .T. ) ;
#8600 = VECTOR ( 'NONE', #7763, 1000.000000000000000 ) ;
#8601 = CARTESIAN_POINT ( 'NONE',  ( 0.000000000000000000, 0.000000000000000000, 0.000000000000000000 ) ) ;
#8602 = CARTESIAN_POINT ( 'NONE',  ( -34.05750781543319050, -36.15000000000000568, -7.963307464738194952 ) ) ;
#8603 = ADVANCED_FACE ( 'NONE', ( #8070 ), #6327, .F. ) ;
#8604 = CARTESIAN_POINT ( 'NONE',  ( -22.93678734525658314, -48.75000000000000711, -7.063212654743582064 ) ) ;
#8605 = CARTESIAN_POINT ( 'NONE',  ( 0.000000000000000000, 0.000000000000000000, 0.000000000000000000 ) ) ;
#8606 = EDGE_LOOP ( 'NONE', ( #3084, #6768, #5349 ) ) ;
#8607 = CARTESIAN_POINT ( 'NONE',  ( -36.28032828410546529, -51.24859572486943193, 6.359104887540839357 ) ) ;
#8608 = CARTESIAN_POINT ( 'NONE',  ( -38.46456197978948666, -35.40000000000000568, 4.312909747525784709 ) ) ;
#8609 = CARTESIAN_POINT ( 'NONE',  ( -22.40239342223677355, -41.90140427513058086, -3.811716262761597473 ) ) ;
#8610 = EDGE_CURVE ( 'NONE', #6319, #5143, #954, .T. ) ;
#8611 =( BOUNDED_CURVE ( )  B_SPLINE_CURVE ( 2, ( #910, #7522, #2288, #3606, #2948, #7438, #6767, #2818, #3480 ),
 .UNSPECIFIED., .F., .T. ) 
 B_SPLINE_CURVE_WITH_KNOTS ( ( 3, 2, 2, 2, 3 ),
 ( 0.07142857142857131358, 0.08928571428571420443, 0.1071428571428570814, 0.1249999999999999722, 0.1428571428571428492 ),
 .UNSPECIFIED. ) 
 CURVE ( )  GEOMETRIC_REPRESENTATION_ITEM ( )  RATIONAL_B_SPLINE_CURVE ( ( 1.000000000000000444, 0.9238795325112862944, 1.000000000000000000, 0.9238795325112867385, 1.000000000000000000, 0.9238795325112867385, 1.000000000000000000, 0.9238795325112867385, 1.000000000000000000 ) ) 
 REPRESENTATION_ITEM ( '' )  );
#8612 = CARTESIAN_POINT ( 'NONE',  ( 0.000000000000000000, -0.8865213383406729264, -1.535499999999999421 ) ) ;
#8613 = CARTESIAN_POINT ( 'NONE',  ( 34.99999999999996447, -44.67046583110982994, 11.45643923738957426 ) ) ;
#8614 = CARTESIAN_POINT ( 'NONE',  ( -37.02382435302582309, -42.24859572486943904, 7.102600956461226467 ) ) ;
#8615 = CARTESIAN_POINT ( 'NONE',  ( -28.43739315969223824, -42.44999999999999574, -9.865911304835512041 ) ) ;
#8616 = VECTOR ( 'NONE', #2018, 1000.000000000000000 ) ;
#8617 = DIRECTION ( 'NONE',  ( 1.000000000000000000, 0.000000000000000000, 0.000000000000000000 ) ) ;
#8618 = CARTESIAN_POINT ( 'NONE',  ( -33.35889894354067309, 8.000000000000000000, 125.0000000000000000 ) ) ;
#8619 = CARTESIAN_POINT ( 'NONE',  ( 3.229347689422841228, -48.22934768942280925, -99.14999999890751781 ) ) ;
#8620 = AXIS2_PLACEMENT_3D ( 'NONE', #6222, #5602, #7627 ) ;
#8621 = EDGE_LOOP ( 'NONE', ( #7342, #6975 ) ) ;
#8622 = DIRECTION ( 'NONE',  ( -0.000000000000000000, -0.000000000000000000, -1.000000000000000000 ) ) ;
#8623 = CARTESIAN_POINT ( 'NONE',  ( -36.28032828410546529, -51.24859572486943193, 6.359104887540839357 ) ) ;
#8624 = CARTESIAN_POINT ( 'NONE',  ( -25.63988726744978663, -35.60140427513057659, -8.440510857627391061 ) ) ;
#8625 = VERTEX_POINT ( 'NONE', #2127 ) ;
#8626 = ORIENTED_EDGE ( 'NONE', *, *, #2573, .T. ) ;
#8627 = AXIS2_PLACEMENT_3D ( 'NONE', #862, #3604, #5489 ) ;
#8628 = CARTESIAN_POINT ( 'NONE',  ( -28.38237549136062654, -47.45140427513057091, -9.857197362228843573 ) ) ;
#8629 = LINE ( 'NONE', #1805, #5112 ) ;
#8630 = CARTESIAN_POINT ( 'NONE',  ( 30.00000000000000000, -49.99999999999997158, -12.49999999999998046 ) ) ;
#8631 = CARTESIAN_POINT ( 'NONE',  ( -3.535533905932735532, -48.53553390593270933, -100.3999999978150441 ) ) ;
#8632 = CARTESIAN_POINT ( 'NONE',  ( 2.000000000000000000, 0.000000000000000000, 0.000000000000000000 ) ) ;
#8633 = CARTESIAN_POINT ( 'NONE',  ( -4.999999999999998224, -44.99999999999997158, -99.00000000000000000 ) ) ;
#8634 = MANIFOLD_SOLID_BREP ( 'Thread1', #1817 ) ;
#8635 = ORIENTED_EDGE ( 'NONE', *, *, #6513, .T. ) ;
#8636 = CARTESIAN_POINT ( 'NONE',  ( -34.05750781543318340, -39.14999999999999147, -7.963307464738195840 ) ) ;
#8637 = ADVANCED_FACE ( 'NONE', ( #6738, #6080 ), #790, .F. ) ;
#8638 = ORIENTED_EDGE ( 'NONE', *, *, #5294, .F. ) ;
#8639 = LINE ( 'NONE', #1685, #1060 ) ;
#8640 = CARTESIAN_POINT ( 'NONE',  ( -3.535533905932736864, -41.46446609406723383, -99.90000000000000568 ) ) ;
#8641 = CARTESIAN_POINT ( 'NONE',  ( -39.38303923565386100, -44.70000000000000284, -1.486127417882099788 ) ) ;
#8642 = CARTESIAN_POINT ( 'NONE',  ( 3.229347689422839895, -41.77065231057713390, -97.94999999890751496 ) ) ;
#8643 = CARTESIAN_POINT ( 'NONE',  ( -1.377418269645616311, -49.84141567902239700, -99.99942299408148472 ) ) ;
#8644 = CARTESIAN_POINT ( 'NONE',  ( -28.54686042191934092, -38.45140427513057801, -8.818680382772479120 ) ) ;
#8645 = AXIS2_PLACEMENT_3D ( 'NONE', #8182, #7592, #5562 ) ;
#8646 = CARTESIAN_POINT ( 'NONE',  ( 3.535533905932736420, -41.46446609406723383, -97.69300000002183992 ) ) ;
#8647 = CARTESIAN_POINT ( 'NONE',  ( -21.17260567462091103, -40.05000000000001137, -1.398121909749241887 ) ) ;
#8648 = FACE_OUTER_BOUND ( 'NONE', #2898, .T. ) ;
#8649 = EDGE_CURVE ( 'NONE', #1675, #7609, #3492, .T. ) ;
#8650 = CARTESIAN_POINT ( 'NONE',  ( -25.68709025247441602, -45.60000000000000853, -8.464561979789547053 ) ) ;
#8651 = DIRECTION ( 'NONE',  ( 0.000000000000000000, 0.000000000000000000, 1.000000000000000000 ) ) ;
#8652 = VERTEX_POINT ( 'NONE', #3778 ) ;
#8653 = FACE_OUTER_BOUND ( 'NONE', #234, .T. ) ;
#8654 = CARTESIAN_POINT ( 'NONE',  ( -38.90016716647221529, -35.84999999999998721, -4.534861676072185155 ) ) ;
#8655 = CARTESIAN_POINT ( 'NONE',  ( -31.39812190974910422, -31.95000000000000639, 8.827394325379140483 ) ) ;
#8656 = CARTESIAN_POINT ( 'NONE',  ( -49.99999999999997158, -59.99999999999997158, 30.00000000000000000 ) ) ;
#8657 = DIRECTION ( 'NONE',  ( -1.000000000000000000, 0.000000000000000000, -0.000000000000000000 ) ) ;
#8658 = CARTESIAN_POINT ( 'NONE',  ( -36.75497492228666374, -33.99859572486943904, -6.680053920257780220 ) ) ;
#8659 = SPHERICAL_SURFACE ( 'NONE', #1978, 1.000000000000000000 ) ;
#8660 = DIRECTION ( 'NONE',  ( -1.000000000000000000, 0.000000000000000000, 0.000000000000000000 ) ) ;
#8661 = CARTESIAN_POINT ( 'NONE',  ( -3.229347689422839451, -48.22934768942280925, -99.34999999890752065 ) ) ;
#8662 = ORIENTED_EDGE ( 'NONE', *, *, #3777, .T. ) ;
#8663 = CARTESIAN_POINT ( 'NONE',  ( -26.64110105645932336, 8.000000000000000000, 124.0000000000000000 ) ) ;
#8664 = CARTESIAN_POINT ( 'NONE',  ( -21.18131961722757595, -32.04859572486944330, -1.453139578080854699 ) ) ;
#8665 = CARTESIAN_POINT ( 'NONE',  ( -39.39132668755255651, -33.69859572486942767, -1.433802505903950308 ) ) ;
#8666 = CARTESIAN_POINT ( 'NONE',  ( -21.12512167993187973, -36.35140427513057659, 4.584493831696868860 ) ) ;
#8667 = ORIENTED_EDGE ( 'NONE', *, *, #2313, .T. ) ;
#8668 = VERTEX_POINT ( 'NONE', #7084 ) ;
#8669 = CARTESIAN_POINT ( 'NONE',  ( -35.97294713907137975, -29.00140427513058583, -6.047868141099968398 ) ) ;
#8670 = DIRECTION ( 'NONE',  ( 1.000000000000000000, 0.000000000000000000, 0.000000000000000000 ) ) ;
#8671 = CARTESIAN_POINT ( 'NONE',  ( -11.32499999999999929, 0.000000000000000000, 0.000000000000000000 ) ) ;
#8672 = CARTESIAN_POINT ( 'NONE',  ( 3.535533905932737309, -48.53553390593270933, -99.39999999781504414 ) ) ;
#8673 = CARTESIAN_POINT ( 'NONE',  ( 30.00000000000001421, -49.99999999999997158, 12.49999999999995914 ) ) ;
#8674 = CARTESIAN_POINT ( 'NONE',  ( 42.00000000000000711, -21.99999999999992184, 60.00000000000002842 ) ) ;
#8675 = EDGE_LOOP ( 'NONE', ( #1296, #8510, #6878, #1213, #2430 ) ) ;
#8676 = CARTESIAN_POINT ( 'NONE',  ( -22.42644454439892598, -45.90000000000001279, -3.858919247786222861 ) ) ;
#8677 = ORIENTED_EDGE ( 'NONE', *, *, #5775, .T. ) ;
#8678 = CARTESIAN_POINT ( 'NONE',  ( 4.566987299999998307, -43.10829192115428299, -98.99999999890751212 ) ) ;
#8679 = CARTESIAN_POINT ( 'NONE',  ( -2.071067811865475505, -49.99999999999996447, -97.14999999781504414 ) ) ;
#8680 = CARTESIAN_POINT ( 'NONE',  ( -37.06321265474346660, -47.25000000000000711, 7.063212654743582952 ) ) ;
#8681 = CARTESIAN_POINT ( 'NONE',  ( -4.566987299999998307, -44.99999999999997158, -96.84999999890753486 ) ) ;
#8682 = CARTESIAN_POINT ( 'NONE',  ( -3.966436988140349396, -41.94266538335023142, -100.0008128833833894 ) ) ;
#8683 = CARTESIAN_POINT ( 'NONE',  ( -26.09387776718931917, -38.60140427513057659, -7.549504333439021941 ) ) ;
#8684 = AXIS2_PLACEMENT_3D ( 'NONE', #7170, #1131, #2386 ) ;
#8685 = CARTESIAN_POINT ( 'NONE',  ( -4.999999999999997335, -47.07106781186546129, -96.54300000002183424 ) ) ;
#8686 = CARTESIAN_POINT ( 'NONE',  ( -21.60464910494133406, -34.20000000000000995, 1.329692952841886155 ) ) ;
#8687 = DIRECTION ( 'NONE',  ( -1.000000000000000000, 0.000000000000000000, 0.000000000000000000 ) ) ;
#8688 = CARTESIAN_POINT ( 'NONE',  ( -21.53543802021056663, -45.90000000000001279, -4.312909747525783821 ) ) ;
#8689 = DIRECTION ( 'NONE',  ( 1.000000000000000000, 0.000000000000000000, 0.000000000000000000 ) ) ;
#8690 = ORIENTED_EDGE ( 'NONE', *, *, #5229, .F. ) ;
#8691 = FACE_OUTER_BOUND ( 'NONE', #5085, .T. ) ;
#8692 = CARTESIAN_POINT ( 'NONE',  ( -28.51387258211773812, -43.80000000000000426, 9.383039235653802379 ) ) ;
#8693 = CARTESIAN_POINT ( 'NONE',  ( -22.06198138166579170, -48.35140427513057659, 4.107139971057695682 ) ) ;
#8694 = FACE_OUTER_BOUND ( 'NONE', #2680, .T. ) ;
#8695 = CARTESIAN_POINT ( 'NONE',  ( -33.35889894354067309, 8.000000000000000000, 124.0000000000000000 ) ) ;
#8696 = CARTESIAN_POINT ( 'NONE',  ( -20.14280263777121149, -38.04859572486944330, -1.617624508639600833 ) ) ;
#8697 = EDGE_CURVE ( 'NONE', #344, #3552, #3734, .T. ) ;
#8698 = CYLINDRICAL_SURFACE ( 'NONE', #7888, 3.500000000000000000 ) ;
#8699 = CARTESIAN_POINT ( 'NONE',  ( -30.00000000000000000, 60.00000000000002842, 0.000000000000000000 ) ) ;
#8700 = CARTESIAN_POINT ( 'NONE',  ( 3.229347689422839895, -41.77065231057713390, -99.74999999890751212 ) ) ;
#8701 = ORIENTED_EDGE ( 'NONE', *, *, #911, .T. ) ;
#8702 = FACE_OUTER_BOUND ( 'NONE', #7976, .T. ) ;
#8703 = CARTESIAN_POINT ( 'NONE',  ( -21.59636165304264921, -32.19859572486942767, 1.277368040863740228 ) ) ;
#8704 = CARTESIAN_POINT ( 'NONE',  ( -28.46154767013959486, -35.79859572486943620, 9.374751783755112200 ) ) ;
#8705 = CARTESIAN_POINT ( 'NONE',  ( -21.51138689804841420, -44.90140427513058086, -4.265706762501151772 ) ) ;
#8706 = ADVANCED_FACE ( 'NONE', ( #1041, #292 ), #5799, .T. ) ;
#8707 = ORIENTED_EDGE ( 'NONE', *, *, #3311, .F. ) ;
#8708 = ORIENTED_EDGE ( 'NONE', *, *, #1464, .T. ) ;
#8709 = CARTESIAN_POINT ( 'NONE',  ( -38.48861310195163554, -49.40140427513058086, 4.265706762501153548 ) ) ;
#8710 = DIRECTION ( 'NONE',  ( 1.000000000000000000, 0.000000000000000000, 0.000000000000000000 ) ) ;
#8711 = CARTESIAN_POINT ( 'NONE',  ( 4.999999999999998224, -44.99999999999997158, -97.69999999781505551 ) ) ;
#8712 = CARTESIAN_POINT ( 'NONE',  ( 2.071067811865477282, -49.99999999999996447, -100.2499999978150669 ) ) ;
#8713 = CARTESIAN_POINT ( 'NONE',  ( -40.00000000000002842, 1.224646799147353059E-15, -44.00000000000000000 ) ) ;
#8714 = CARTESIAN_POINT ( 'NONE',  ( -4.999999999999998224, -44.99999999999997158, -98.19999999999998863 ) ) ;
#8715 = ORIENTED_EDGE ( 'NONE', *, *, #5502, .T. ) ;
#8716 = EDGE_CURVE ( 'NONE', #6772, #7413, #1603, .T. ) ;
#8717 = DIRECTION ( 'NONE',  ( -1.000000000000000000, 0.000000000000000000, 0.000000000000000000 ) ) ;
#8718 = NEXT_ASSEMBLY_USAGE_OCCURRENCE ( 'NAUO1', ' ', ' ', #2226, #2881, $ ) ;
#8719 = NEXT_ASSEMBLY_USAGE_OCCURRENCE ( 'NAUO2', ' ', ' ', #2226, #1576, $ ) ;
#8720 = NEXT_ASSEMBLY_USAGE_OCCURRENCE ( 'NAUO3', ' ', ' ', #2226, #5889, $ ) ;
#8721 = NEXT_ASSEMBLY_USAGE_OCCURRENCE ( 'NAUO4', ' ', ' ', #2226, #4320, $ ) ;
#8722 = NEXT_ASSEMBLY_USAGE_OCCURRENCE ( 'NAUO5', ' ', ' ', #2226, #4320, $ ) ;
#8723 = NEXT_ASSEMBLY_USAGE_OCCURRENCE ( 'NAUO6', ' ', ' ', #2226, #5874, $ ) ;
#8724 = NEXT_ASSEMBLY_USAGE_OCCURRENCE ( 'NAUO7', ' ', ' ', #2226, #6796, $ ) ;
#8725 = NEXT_ASSEMBLY_USAGE_OCCURRENCE ( 'NAUO8', ' ', ' ', #2226, #1843, $ ) ;
#8726 = NEXT_ASSEMBLY_USAGE_OCCURRENCE ( 'NAUO9', ' ', ' ', #2226, #1843, $ ) ;
#8727 = NEXT_ASSEMBLY_USAGE_OCCURRENCE ( 'NAUO10', ' ', ' ', #2226, #1843, $ ) ;
#8728 = NEXT_ASSEMBLY_USAGE_OCCURRENCE ( 'NAUO11', ' ', ' ', #2226, #1843, $ ) ;
#8729 = NEXT_ASSEMBLY_USAGE_OCCURRENCE ( 'NAUO12', ' ', ' ', #2226, #5889, $ ) ;
#8730 = NEXT_ASSEMBLY_USAGE_OCCURRENCE ( 'NAUO13', ' ', ' ', #2226, #5874, $ ) ;
#8731 = NEXT_ASSEMBLY_USAGE_OCCURRENCE ( 'NAUO14', ' ', ' ', #2226, #4320, $ ) ;
#8732 = NEXT_ASSEMBLY_USAGE_OCCURRENCE ( 'NAUO15', ' ', ' ', #2226, #4320, $ ) ;
#8733 = NEXT_ASSEMBLY_USAGE_OCCURRENCE ( 'NAUO16', ' ', ' ', #2226, #6796, $ ) ;
ENDSEC;
END-ISO-10303-21;
